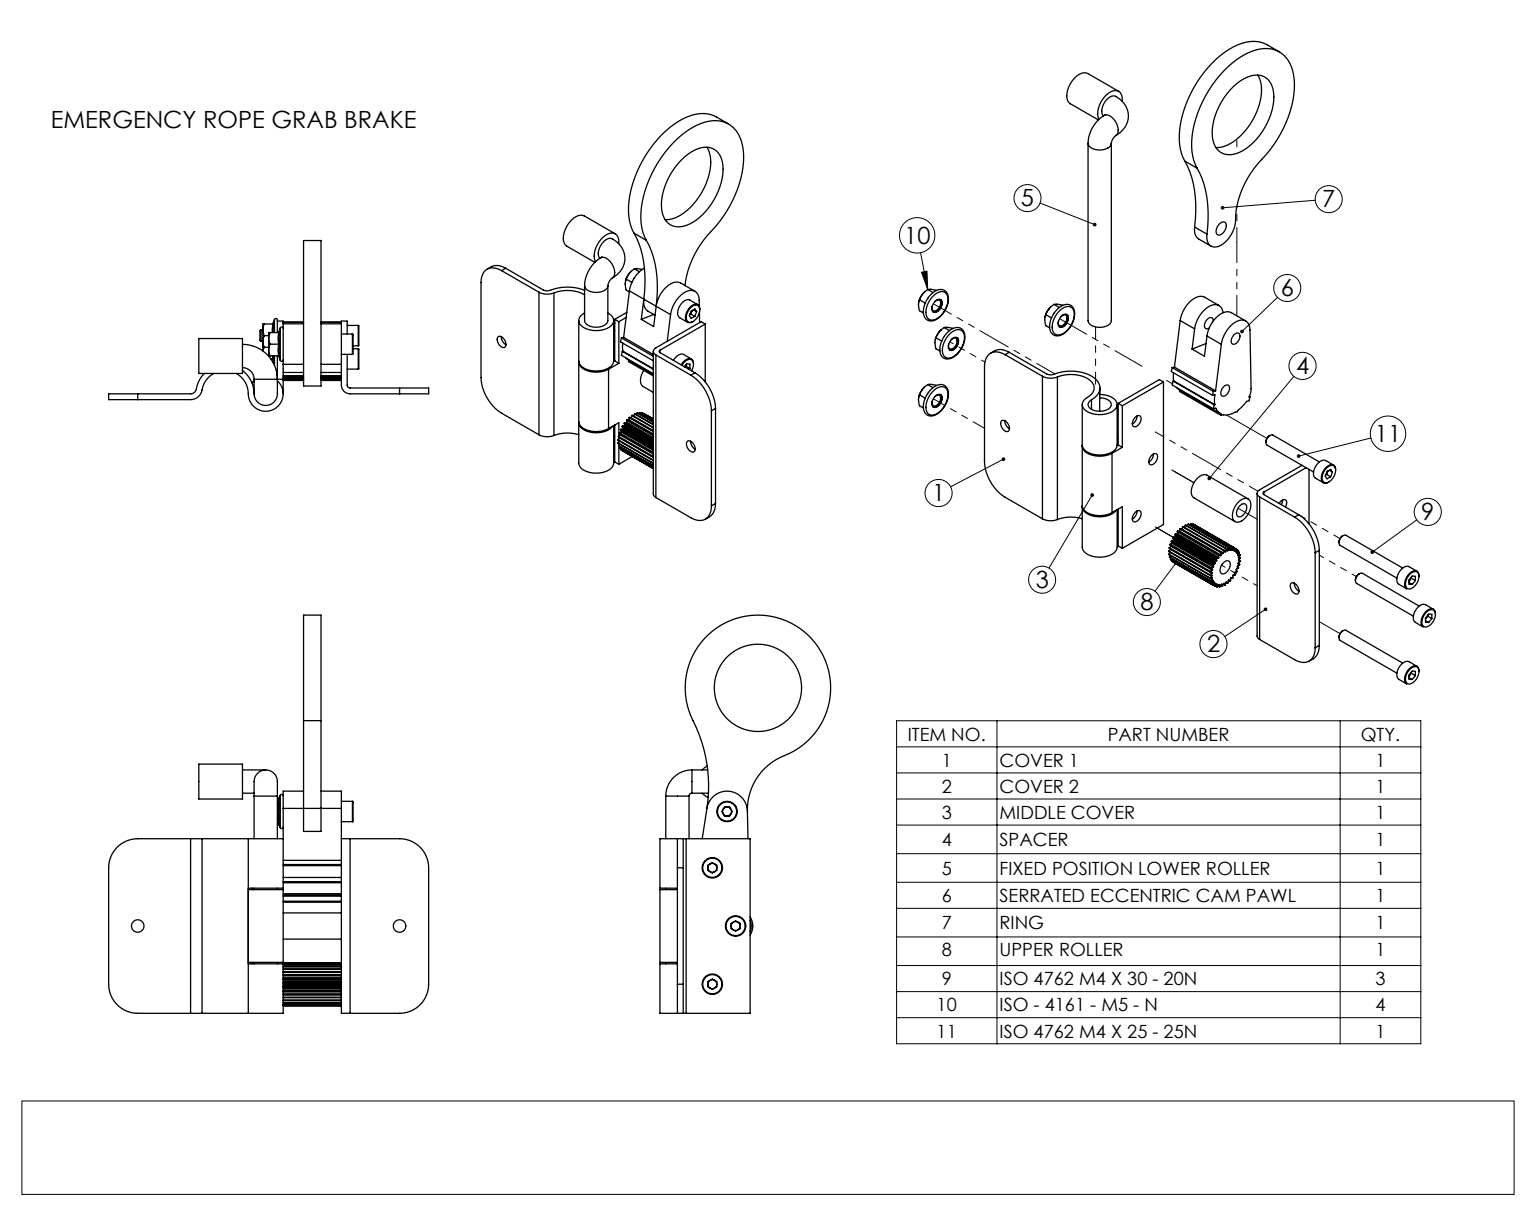
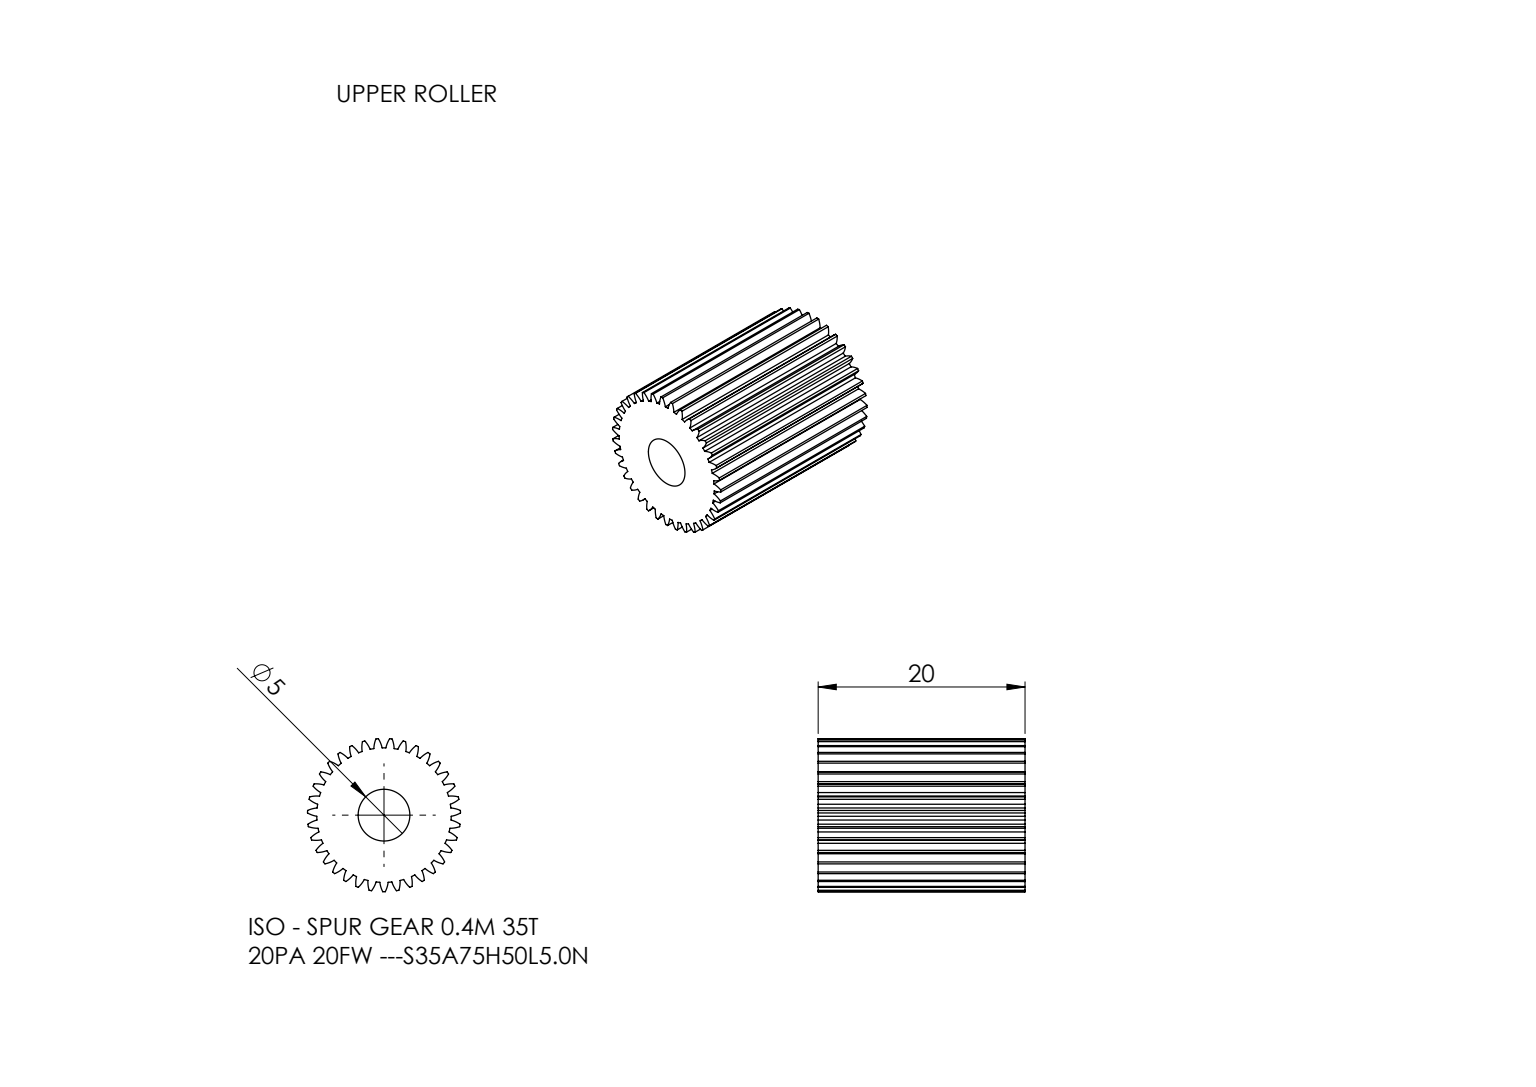
ISO-10303-21;
HEADER;
FILE_DESCRIPTION (('STEP AP214'),
    '1' );
FILE_NAME ('BR-598',
    '2026-10-03T20:08:58',
    ( '' ),
    ( '' ),
    'SwSTEP 2.0',
    'SolidWorks 2026',
    '' );
FILE_SCHEMA (( 'AUTOMOTIVE_DESIGN' ));
ENDSEC;

DATA;
#1 = FACE_OUTER_BOUND ( 'NONE', #4766, .T. ) ;
#2 = APPLICATION_CONTEXT ( 'automotive_design' ) ;
#3 = ORIENTED_EDGE ( 'NONE', *, *, #5317, .F. ) ;
#4 = CARTESIAN_POINT ( 'NONE',  ( 34.00000000000000000, 0.000000000000000000, -1.734723475976807094E-14 ) ) ;
#5 = ORIENTED_EDGE ( 'NONE', *, *, #5789, .T. ) ;
#6 = CARTESIAN_POINT ( 'NONE',  ( 33.00000000000001421, 39.34792583643766761, -10.06347054209568270 ) ) ;
#7 = AXIS2_PLACEMENT_3D ( 'NONE', #1534, #4440, #9440 ) ;
#9 = AXIS2_PLACEMENT_3D ( 'NONE', #3779, #3718, #5895 ) ;
#8 = SHAPE_REPRESENTATION_RELATIONSHIP ( 'NONE' , 'NONE' ,  #10094, #6187 ) ;
#10 = VECTOR ( 'NONE', #8821, 1000.000000000000000 ) ;
#11 = ADVANCED_FACE ( 'NONE', ( #11750 ), #8898, .T. ) ;
#12 = CARTESIAN_POINT ( 'NONE',  ( 19.99999999999997868, 5.670261409740700920, -3.175710400084609475 ) ) ;
#13 = CARTESIAN_POINT ( 'NONE',  ( 9.999999999999994671, -7.399010254356641170, 0.1210258481698957278 ) ) ;
#14 = FACE_OUTER_BOUND ( 'NONE', #4864, .T. ) ;
#15 = PLANE ( 'NONE',  #8371 ) ;
#16 = CARTESIAN_POINT ( 'NONE',  ( -3.999999999999991562, -0.3979232138631201288, 7.067642911889882029E-15 ) ) ;
#17 = DIRECTION ( 'NONE',  ( 0.000000000000000000, 0.000000000000000000, 1.000000000000000000 ) ) ;
#18 = DIRECTION ( 'NONE',  ( 1.140150527077241873E-30, 0.000000000000000000, -1.000000000000000000 ) ) ;
#19 = FACE_OUTER_BOUND ( 'NONE', #8393, .T. ) ;
#20 =( GEOMETRIC_REPRESENTATION_CONTEXT ( 3 ) GLOBAL_UNCERTAINTY_ASSIGNED_CONTEXT ( ( #3670 ) ) GLOBAL_UNIT_ASSIGNED_CONTEXT ( ( #5671, #4709, #1872 ) ) REPRESENTATION_CONTEXT ( 'NONE', 'WORKASPACE' ) );
#21 = ORIENTED_EDGE ( 'NONE', *, *, #12558, .T. ) ;
#22 = DIRECTION ( 'NONE',  ( -1.000000000000000000, 1.010728034814421376E-30, 1.090846720500930387E-30 ) ) ;
#23 = EDGE_CURVE ( 'NONE', #11067, #11603, #10115, .T. ) ;
#24 = LINE ( 'NONE', #10641, #9116 ) ;
#25 = CARTESIAN_POINT ( 'NONE',  ( 4.000000000000000000, -0.7890432684750908754, -0.04868663549882277369 ) ) ;
#27 = ADVANCED_FACE ( 'NONE', ( #3005 ), #10828, .T. ) ;
#26 = DIRECTION ( 'NONE',  ( 0.000000000000000000, 0.000000000000000000, 1.000000000000000000 ) ) ;
#28 = CARTESIAN_POINT ( 'NONE',  ( 19.99999999999999645, 0.000000000000000000, 0.000000000000000000 ) ) ;
#29 = ORIENTED_EDGE ( 'NONE', *, *, #11225, .F. ) ;
#30 = LINE ( 'NONE', #10838, #312 ) ;
#31 = CARTESIAN_POINT ( 'NONE',  ( 0.000000000000000000, -6.884685972239682705, 2.713134545806031195 ) ) ;
#32 = AXIS2_PLACEMENT_3D ( 'NONE', #10637, #3883, #7557 ) ;
#33 = DIRECTION ( 'NONE',  ( 1.000000000000000000, 1.081682119347366321E-16, -5.551115123125780237E-17 ) ) ;
#34 = ORIENTED_EDGE ( 'NONE', *, *, #4126, .T. ) ;
#35 = VERTEX_POINT ( 'NONE', #4203 ) ;
#36 = CARTESIAN_POINT ( 'NONE',  ( -3.333333333333346804, 2.694301256218253560, -3.300726591567095358 ) ) ;
#37 = ORIENTED_EDGE ( 'NONE', *, *, #5489, .T. ) ;
#38 = VERTEX_POINT ( 'NONE', #7300 ) ;
#39 = SHAPE_DEFINITION_REPRESENTATION ( #2484, #8378 ) ;
#40 = LINE ( 'NONE', #5122, #406 ) ;
#41 = VERTEX_POINT ( 'NONE', #145 ) ;
#42 = AXIS2_PLACEMENT_3D ( 'NONE', #12709, #3754, #3875 ) ;
#43 = FILL_AREA_STYLE ('',( #2962 ) ) ;
#44 = PLANE ( 'NONE',  #3777 ) ;
#45 = AXIS2_PLACEMENT_3D ( 'NONE', #142, #4066, #10040 ) ;
#46 = EDGE_CURVE ( 'NONE', #9407, #3079, #7991, .T. ) ;
#47 = VERTEX_POINT ( 'NONE', #5047 ) ;
#48 = DIRECTION ( 'NONE',  ( -0.000000000000000000, -1.000000000000000000, -0.000000000000000000 ) ) ;
#49 = CARTESIAN_POINT ( 'NONE',  ( 19.99999999999999645, -6.484265599627176968, 1.105616797298907716 ) ) ;
#50 = ORIENTED_EDGE ( 'NONE', *, *, #4393, .F. ) ;
#51 = ORIENTED_EDGE ( 'NONE', *, *, #132, .F. ) ;
#52 = AXIS2_PLACEMENT_3D ( 'NONE', #7977, #7092, #2061 ) ;
#53 = ORIENTED_EDGE ( 'NONE', *, *, #9830, .F. ) ;
#54 = DIRECTION ( 'NONE',  ( 7.272311470006191196E-31, 0.3513748240813434620, -0.9362348706397368714 ) ) ;
#55 = ORIENTED_EDGE ( 'NONE', *, *, #6653, .F. ) ;
#56 = ADVANCED_FACE ( 'NONE', ( #4070, #400 ), #9089, .T. ) ;
#57 = CARTESIAN_POINT ( 'NONE',  ( 19.99999999999999645, 0.000000000000000000, 0.000000000000000000 ) ) ;
#58 = ORIENTED_EDGE ( 'NONE', *, *, #11138, .F. ) ;
#59 = EDGE_CURVE ( 'NONE', #992, #4885, #7267, .T. ) ;
#60 = VECTOR ( 'NONE', #10370, 1000.000000000000000 ) ;
#61 = VECTOR ( 'NONE', #3554, 1000.000000000000000 ) ;
#62 = EDGE_CURVE ( 'NONE', #1807, #9471, #2410, .T. ) ;
#63 = CARTESIAN_POINT ( 'NONE',  ( 14.00000000000000000, 12.99999999999999822, 0.000000000000000000 ) ) ;
#64 = DIRECTION ( 'NONE',  ( -1.000000000000000000, 1.010728034814421376E-30, 1.090846720500930387E-30 ) ) ;
#65 = EDGE_CURVE ( 'NONE', #6211, #2771, #7241, .T. ) ;
#66 = EDGE_LOOP ( 'NONE', ( #746, #6032, #7828, #1571 ) ) ;
#67 = DIRECTION ( 'NONE',  ( -1.000000000000000000, 1.010728034814421376E-30, 1.090846720500930387E-30 ) ) ;
#68 = CIRCLE ( 'NONE', #2542, 6.499000000000009436 ) ;
#69 = ORIENTED_EDGE ( 'NONE', *, *, #11638, .T. ) ;
#70 = DIRECTION ( 'NONE',  ( 0.000000000000000000, 0.000000000000000000, 1.000000000000000000 ) ) ;
#71 = SHAPE_REPRESENTATION ( 'middle cover', ( #12422 ), #3113 ) ;
#72 = CARTESIAN_POINT ( 'NONE',  ( 2.000000000000001776, 1.773042676681341856, -3.469446951953614189E-15 ) ) ;
#73 = CARTESIAN_POINT ( 'NONE',  ( 19.99999999999999645, -2.385831757338583881, 6.045230171438861433 ) ) ;
#74 = VECTOR ( 'NONE', #10959, 1000.000000000000000 ) ;
#75 = CARTESIAN_POINT ( 'NONE',  ( -11.83215956619923226, -30.00000000000000000, -4.336808689942017736E-16 ) ) ;
#76 = CARTESIAN_POINT ( 'NONE',  ( -2.000000000000008882, -3.464101615137750390, -8.673617379884035472E-15 ) ) ;
#77 = DIRECTION ( 'NONE',  ( 0.000000000000000000, 0.000000000000000000, 1.000000000000000000 ) ) ;
#78 = CARTESIAN_POINT ( 'NONE',  ( 19.99999999999997868, -2.171317488608451196, -7.074275960383738848 ) ) ;
#79 = LINE ( 'NONE', #4007, #1843 ) ;
#80 = CARTESIAN_POINT ( 'NONE',  ( -16.99999999999999289, 30.00000000000000000, 25.00000000000007105 ) ) ;
#81 = AXIS2_PLACEMENT_3D ( 'NONE', #653, #10630, #1876 ) ;
#82 = ORIENTED_EDGE ( 'NONE', *, *, #340, .T. ) ;
#83 = ORIENTED_EDGE ( 'NONE', *, *, #1095, .T. ) ;
#84 = CARTESIAN_POINT ( 'NONE',  ( 3.469446951953614189E-14, -3.469446951953614189E-15, -4.694516984716123886 ) ) ;
#85 = FACE_OUTER_BOUND ( 'NONE', #4807, .T. ) ;
#86 = LINE ( 'NONE', #3133, #9986 ) ;
#87 = VERTEX_POINT ( 'NONE', #3260 ) ;
#88 = AXIS2_PLACEMENT_3D ( 'NONE', #6205, #12269, #12210 ) ;
#89 = EDGE_CURVE ( 'NONE', #11132, #9471, #8961, .T. ) ;
#90 = FACE_OUTER_BOUND ( 'NONE', #10199, .T. ) ;
#91 = LINE ( 'NONE', #9864, #6054 ) ;
#92 = CARTESIAN_POINT ( 'NONE',  ( 40.00000000000006395, 1.290960574571364216E-15, -20.00000000000000000 ) ) ;
#93 = VERTEX_POINT ( 'NONE', #9152 ) ;
#94 = ORIENTED_EDGE ( 'NONE', *, *, #6721, .T. ) ;
#95 = CARTESIAN_POINT ( 'NONE',  ( 20.00000000000000000, 39.49790820824818383, -24.06186359251417883 ) ) ;
#96 = EDGE_LOOP ( 'NONE', ( #11303, #3914, #11621, #9750 ) ) ;
#97 = AXIS2_PLACEMENT_3D ( 'NONE', #1483, #11545, #8437 ) ;
#98 = ORIENTED_EDGE ( 'NONE', *, *, #5230, .F. ) ;
#99 = SHAPE_DEFINITION_REPRESENTATION ( #6268, #1377 ) ;
#100 = DIRECTION ( 'NONE',  ( 0.000000000000000000, -0.9909497617679331460, -0.1342332658176667304 ) ) ;
#101 = ORIENTED_EDGE ( 'NONE', *, *, #1479, .F. ) ;
#102 = DIRECTION ( 'NONE',  ( -1.000000000000000000, 1.010728034814421376E-30, 1.090846720500930387E-30 ) ) ;
#103 = ORIENTED_EDGE ( 'NONE', *, *, #2776, .T. ) ;
#104 = FACE_OUTER_BOUND ( 'NONE', #9795, .T. ) ;
#105 = CARTESIAN_POINT ( 'NONE',  ( 9.999999999999994671, -7.301715115245761112, -1.202063382601588959 ) ) ;
#106 = CONICAL_SURFACE ( 'NONE', #7315, 1.535500000000000087, 1.047197551196590748 ) ;
#107 = CIRCLE ( 'NONE', #5659, 4.000000000000001776 ) ;
#108 = ORIENTED_EDGE ( 'NONE', *, *, #10644, .F. ) ;
#109 = ADVANCED_FACE ( 'NONE', ( #2146 ), #3325, .T. ) ;
#110 = ORIENTED_EDGE ( 'NONE', *, *, #895, .F. ) ;
#111 = EDGE_CURVE ( 'NONE', #3787, #7514, #12202, .T. ) ;
#112 = EDGE_CURVE ( 'NONE', #3836, #11042, #11228, .T. ) ;
#113 = ORIENTED_EDGE ( 'NONE', *, *, #3942, .T. ) ;
#114 = DIRECTION ( 'NONE',  ( -1.000000000000000000, 1.010728034814421376E-30, 1.090846720500930387E-30 ) ) ;
#115 = DIRECTION ( 'NONE',  ( 0.000000000000000000, -1.530455820933490821E-32, 1.000000000000000000 ) ) ;
#116 = ORIENTED_EDGE ( 'NONE', *, *, #9811, .T. ) ;
#117 = AXIS2_PLACEMENT_3D ( 'NONE', #8062, #12074, #12010 ) ;
#118 = DIRECTION ( 'NONE',  ( 1.238279320584846685E-16, -0.9554649393887558739, 0.2951046417778634412 ) ) ;
#119 = ORIENTED_EDGE ( 'NONE', *, *, #7545, .T. ) ;
#120 = EDGE_CURVE ( 'NONE', #10609, #7454, #4588, .T. ) ;
#121 = FACE_OUTER_BOUND ( 'NONE', #12151, .T. ) ;
#122 = CARTESIAN_POINT ( 'NONE',  ( 19.99999999999999645, -5.610543508060446882, 3.433640984893234549 ) ) ;
#123 = CARTESIAN_POINT ( 'NONE',  ( 19.99999999999999645, -4.155687294075553595, -5.098857909653601084 ) ) ;
#124 = VECTOR ( 'NONE', #5391, 1000.000000000000000 ) ;
#125 = VERTEX_POINT ( 'NONE', #8190 ) ;
#126 = FACE_OUTER_BOUND ( 'NONE', #189, .T. ) ;
#127 = ORIENTED_EDGE ( 'NONE', *, *, #89, .F. ) ;
#128 = CARTESIAN_POINT ( 'NONE',  ( 19.99999999999999645, 0.000000000000000000, 0.000000000000000000 ) ) ;
#129 = CARTESIAN_POINT ( 'NONE',  ( 9.999999999999998224, 7.100173756228433497, 2.085073771204572157 ) ) ;
#130 = CIRCLE ( 'NONE', #8361, 7.400000000000011902 ) ;
#131 = DIRECTION ( 'NONE',  ( 0.000000000000000000, -1.177425296209236209E-30, -1.000000000000000000 ) ) ;
#132 = EDGE_CURVE ( 'NONE', #3832, #6132, #1903, .T. ) ;
#133 = CIRCLE ( 'NONE', #4662, 7.400000000000011902 ) ;
#134 = CARTESIAN_POINT ( 'NONE',  ( 0.000000000000000000, 4.192831774278975132, 4.965597920955404199 ) ) ;
#135 = CARTESIAN_POINT ( 'NONE',  ( 40.00000000000000711, 9.597108420813798446, -18.39576936187866352 ) ) ;
#136 = DIRECTION ( 'NONE',  ( 1.000000000000000000, 0.000000000000000000, 0.000000000000000000 ) ) ;
#137 = DIRECTION ( 'NONE',  ( 1.000000000000000000, -1.010728034814421376E-30, -1.090846720500930387E-30 ) ) ;
#138 = PRODUCT_DEFINITION_FORMATION_WITH_SPECIFIED_SOURCE ( 'ANY', '', #5241, .NOT_KNOWN. ) ;
#139 = DIRECTION ( 'NONE',  ( 0.000000000000000000, 0.000000000000000000, -1.000000000000000000 ) ) ;
#140 = CIRCLE ( 'NONE', #5087, 10.00000000000002309 ) ;
#141 = ADVANCED_FACE ( 'NONE', ( #9022 ), #11990, .F. ) ;
#142 = CARTESIAN_POINT ( 'NONE',  ( 14.00000000000000000, 13.00000000000000000, 0.000000000000000000 ) ) ;
#143 = EDGE_CURVE ( 'NONE', #5907, #8271, #10318, .T. ) ;
#144 = VERTEX_POINT ( 'NONE', #12137 ) ;
#145 = CARTESIAN_POINT ( 'NONE',  ( 19.99999999999997868, 0.6915992404090851586, -6.462096524400249287 ) ) ;
#146 = CARTESIAN_POINT ( 'NONE',  ( 0.000000000000000000, 4.772487208025128602, 4.411390579991361527 ) ) ;
#147 = CARTESIAN_POINT ( 'NONE',  ( 19.99999999999999645, -5.651611091574833878, 4.776954267060571802 ) ) ;
#148 = CARTESIAN_POINT ( 'NONE',  ( 14.00000000000000000, -13.00000000000000000, 0.000000000000000000 ) ) ;
#149 = CARTESIAN_POINT ( 'NONE',  ( 20.00000000000000355, 19.99999999999999645, -9.850000000000008527 ) ) ;
#150 = ORIENTED_EDGE ( 'NONE', *, *, #8938, .F. ) ;
#151 = CIRCLE ( 'NONE', #11268, 2.800000000000003375 ) ;
#152 = FACE_OUTER_BOUND ( 'NONE', #1535, .T. ) ;
#153 = CYLINDRICAL_SURFACE ( 'NONE', #2365, 2.149999999999999023 ) ;
#154 = EDGE_CURVE ( 'NONE', #6728, #2957, #12005, .T. ) ;
#155 = ORIENTED_EDGE ( 'NONE', *, *, #11867, .F. ) ;
#156 = VERTEX_POINT ( 'NONE', #5173 ) ;
#157 = DIRECTION ( 'NONE',  ( 0.000000000000000000, -1.530455820933490821E-32, 1.000000000000000000 ) ) ;
#158 = ORIENTED_EDGE ( 'NONE', *, *, #7731, .T. ) ;
#159 = ORIENTED_EDGE ( 'NONE', *, *, #9670, .T. ) ;
#160 = APPLICATION_PROTOCOL_DEFINITION ( 'draft international standard', 'automotive_design', 1998, #5024 ) ;
#161 = DIRECTION ( 'NONE',  ( 0.000000000000000000, 0.000000000000000000, 1.000000000000000000 ) ) ;
#162 = ORIENTED_EDGE ( 'NONE', *, *, #10787, .F. ) ;
#163 = CARTESIAN_POINT ( 'NONE',  ( 4.000000000000003553, 1.942890293094023946E-16, 3.500000000000003997 ) ) ;
#164 = EDGE_CURVE ( 'NONE', #2848, #3887, #6852, .T. ) ;
#165 = CARTESIAN_POINT ( 'NONE',  ( 14.00000000000000000, -30.00000000000000000, 0.000000000000000000 ) ) ;
#166 = EDGE_LOOP ( 'NONE', ( #3559, #613, #8519, #6620, #10979 ) ) ;
#167 = CARTESIAN_POINT ( 'NONE',  ( 0.000000000000000000, 4.772487208025201433, -4.411390579991299354 ) ) ;
#168 = DIRECTION ( 'NONE',  ( -1.000000000000000000, 1.010728034814421376E-30, 1.090846720500930387E-30 ) ) ;
#169 =( REPRESENTATION_RELATIONSHIP ('NONE','NONE', #10018, #9199 ) REPRESENTATION_RELATIONSHIP_WITH_TRANSFORMATION ( #7317 )SHAPE_REPRESENTATION_RELATIONSHIP( ) );
#170 = CARTESIAN_POINT ( 'NONE',  ( 20.00000000000000355, 10.25912655421750230, -11.14847175327133577 ) ) ;
#171 = AXIS2_PLACEMENT_3D ( 'NONE', #7633, #11626, #11439 ) ;
#172 = ORIENTED_EDGE ( 'NONE', *, *, #1630, .T. ) ;
#173 = ORIENTED_EDGE ( 'NONE', *, *, #5262, .T. ) ;
#174 = ORIENTED_EDGE ( 'NONE', *, *, #9059, .T. ) ;
#175 = VERTEX_POINT ( 'NONE', #5295 ) ;
#176 = FACE_OUTER_BOUND ( 'NONE', #7657, .T. ) ;
#177 = CARTESIAN_POINT ( 'NONE',  ( 4.203935335434870524, 1.640780671294068238, -3.598452447879444627 ) ) ;
#178 = ORIENTED_EDGE ( 'NONE', *, *, #3075, .F. ) ;
#179 = FACE_OUTER_BOUND ( 'NONE', #3393, .T. ) ;
#180 = CONICAL_SURFACE ( 'NONE', #8811, 4.000000000000000000, 0.8911886515913786111 ) ;
#181 = ORIENTED_EDGE ( 'NONE', *, *, #9473, .F. ) ;
#182 = CARTESIAN_POINT ( 'NONE',  ( 3.122502256758252770E-14, -4.862606272033112909, -3.745885042887444616 ) ) ;
#183 = EDGE_CURVE ( 'NONE', #1508, #4176, #5201, .T. ) ;
#184 = ADVANCED_FACE ( 'NONE', ( #12327 ), #9395, .T. ) ;
#185 = CARTESIAN_POINT ( 'NONE',  ( 15.00000000000003375, -12.49999999999999645, 3.994800001834461867E-31 ) ) ;
#186 = AXIS2_PLACEMENT_3D ( 'NONE', #11743, #4909, #6785 ) ;
#187 = AXIS2_PLACEMENT_3D ( 'NONE', #3419, #6498, #628 ) ;
#188 = FACE_OUTER_BOUND ( 'NONE', #3903, .T. ) ;
#189 = EDGE_LOOP ( 'NONE', ( #7813, #4813, #3733, #12234, #6794, #9118 ) ) ;
#190 = FACE_OUTER_BOUND ( 'NONE', #6817, .T. ) ;
#191 = ORIENTED_EDGE ( 'NONE', *, *, #10270, .T. ) ;
#192 = PLANE ( 'NONE',  #6009 ) ;
#193 =( NAMED_UNIT ( * ) PLANE_ANGLE_UNIT ( ) SI_UNIT ( $, .RADIAN. ) );
#194 = FACE_OUTER_BOUND ( 'NONE', #7754, .T. ) ;
#195 = AXIS2_PLACEMENT_3D ( 'NONE', #7539, #2660, #4452 ) ;
#196 = AXIS2_PLACEMENT_3D ( 'NONE', #1167, #8956, #10887 ) ;
#197 = CIRCLE ( 'NONE', #2043, 2.800000000000002931 ) ;
#198 = DIRECTION ( 'NONE',  ( 1.000000000000000000, 1.849040895279789448E-31, -6.938893903907224680E-17 ) ) ;
#199 = AXIS2_PLACEMENT_3D ( 'NONE', #4415, #11118, #3403 ) ;
#200 = CARTESIAN_POINT ( 'NONE',  ( 2.000000000000001776, 0.000000000000000000, 0.000000000000000000 ) ) ;
#201 = DIRECTION ( 'NONE',  ( 0.000000000000000000, 0.4999999999999989453, -0.8660254037844392627 ) ) ;
#202 = DIRECTION ( 'NONE',  ( -1.000000000000000000, 1.010728034814421376E-30, 1.090846720500930387E-30 ) ) ;
#203 = CARTESIAN_POINT ( 'NONE',  ( 15.00000000000003375, 30.00000000000001776, -9.742497179615118866E-31 ) ) ;
#204 = CIRCLE ( 'NONE', #7, 6.499000000000010324 ) ;
#205 = AXIS2_PLACEMENT_3D ( 'NONE', #5168, #9083, #12128 ) ;
#206 = CARTESIAN_POINT ( 'NONE',  ( 0.000000000000000000, -1.623118704078857499, -6.293050665016890477 ) ) ;
#207 = ORIENTED_EDGE ( 'NONE', *, *, #11487, .T. ) ;
#208 = CARTESIAN_POINT ( 'NONE',  ( 0.000000000000000000, 0.000000000000000000, 0.000000000000000000 ) ) ;
#209 = COLOUR_RGB ( '', 0.66274510, 0.83137255, 0.94901961) ;
#210 = PRESENTATION_LAYER_ASSIGNMENT (  '', '', ( #5766 ) ) ;
#211 = CARTESIAN_POINT ( 'NONE',  ( 27.00000000000000355, 39.34792583643766051, -14.91347054209568945 ) ) ;
#212 = CARTESIAN_POINT ( 'NONE',  ( 2.000000000000001776, -1.773042676681341856, 3.469446951953614189E-15 ) ) ;
#213 = EDGE_CURVE ( 'NONE', #4292, #815, #7867, .T. ) ;
#214 = CARTESIAN_POINT ( 'NONE',  ( 0.000000000000000000, 0.000000000000000000, 0.000000000000000000 ) ) ;
#215 = ORIENTED_EDGE ( 'NONE', *, *, #9401, .F. ) ;
#216 = CARTESIAN_POINT ( 'NONE',  ( 40.00000000000000000, 39.34792583643765340, -17.06347054209567560 ) ) ;
#217 = EDGE_CURVE ( 'NONE', #10195, #4167, #2330, .T. ) ;
#218 = CARTESIAN_POINT ( 'NONE',  ( 2.000000000000001776, -0.8865213383406691516, 1.535500000000002085 ) ) ;
#219 = ORIENTED_EDGE ( 'NONE', *, *, #11430, .T. ) ;
#220 = ADVANCED_FACE ( 'NONE', ( #2602 ), #12455, .T. ) ;
#221 = DIRECTION ( 'NONE',  ( 0.000000000000000000, 0.000000000000000000, 1.000000000000000000 ) ) ;
#222 = VERTEX_POINT ( 'NONE', #588 ) ;
#223 = EDGE_LOOP ( 'NONE', ( #680, #8634, #6232, #8801 ) ) ;
#224 = APPLICATION_PROTOCOL_DEFINITION ( 'draft international standard', 'automotive_design', 1998, #2906 ) ;
#225 = CYLINDRICAL_SURFACE ( 'NONE', #8627, 4.000000000000008882 ) ;
#226 = ORIENTED_EDGE ( 'NONE', *, *, #11853, .T. ) ;
#227 =( NAMED_UNIT ( * ) PLANE_ANGLE_UNIT ( ) SI_UNIT ( $, .RADIAN. ) );
#228 = CARTESIAN_POINT ( 'NONE',  ( 19.99999999999997868, 6.146182963951697609, -2.112211157443803611 ) ) ;
#229 = VERTEX_POINT ( 'NONE', #7547 ) ;
#230 = CARTESIAN_POINT ( 'NONE',  ( 9.999999999999980460, -5.492355906873422455, 4.959236492871922586 ) ) ;
#231 = CARTESIAN_POINT ( 'NONE',  ( 40.00000000000000711, 10.63631887905126128, -9.927230231572499619 ) ) ;
#232 = DIRECTION ( 'NONE',  ( 1.158639454543359513E-30, -0.1785568947986227173, -0.9839295885986321100 ) ) ;
#233 = DIRECTION ( 'NONE',  ( 0.000000000000000000, 0.8660254037844380415, -0.5000000000000012212 ) ) ;
#234 = CIRCLE ( 'NONE', #8869, 6.000000000000000888 ) ;
#235 = VERTEX_POINT ( 'NONE', #4529 ) ;
#236 = ORIENTED_EDGE ( 'NONE', *, *, #12303, .F. ) ;
#237 = EDGE_LOOP ( 'NONE', ( #1805, #3324, #10150, #7771, #10592, #866 ) ) ;
#238 = ORIENTED_EDGE ( 'NONE', *, *, #6687, .T. ) ;
#239 = CIRCLE ( 'NONE', #9478, 4.000000000000001776 ) ;
#240 = DIRECTION ( 'NONE',  ( -4.930380657631325535E-31, -1.000000000000000000, -1.177425296209239362E-30 ) ) ;
#241 = AXIS2_PLACEMENT_3D ( 'NONE', #12258, #11351, #9391 ) ;
#242 = CARTESIAN_POINT ( 'NONE',  ( 0.000000000000000000, 0.000000000000000000, 0.000000000000000000 ) ) ;
#243 = ORIENTED_EDGE ( 'NONE', *, *, #11135, .T. ) ;
#244 = CARTESIAN_POINT ( 'NONE',  ( -10.00000000000000178, 0.000000000000000000, 0.000000000000000000 ) ) ;
#245 = VERTEX_POINT ( 'NONE', #10303 ) ;
#246 = CARTESIAN_POINT ( 'NONE',  ( 19.99999999999999645, -4.155687294075553595, -5.098857909653601084 ) ) ;
#247 = AXIS2_PLACEMENT_3D ( 'NONE', #6312, #11214, #8436 ) ;
#248 = CARTESIAN_POINT ( 'NONE',  ( 0.000000000000000000, 0.000000000000000000, 0.000000000000000000 ) ) ;
#249 = LINE ( 'NONE', #7281, #6377 ) ;
#250 = ORIENTED_EDGE ( 'NONE', *, *, #9565, .F. ) ;
#251 = DIRECTION ( 'NONE',  ( -1.000000000000000000, -0.000000000000000000, -0.000000000000000000 ) ) ;
#252 = ORIENTED_EDGE ( 'NONE', *, *, #804, .T. ) ;
#253 = CARTESIAN_POINT ( 'NONE',  ( 0.000000000000000000, 0.000000000000000000, 0.000000000000000000 ) ) ;
#254 = EDGE_CURVE ( 'NONE', #6132, #11730, #871, .T. ) ;
#255 =( LENGTH_UNIT ( ) NAMED_UNIT ( * ) SI_UNIT ( .MILLI., .METRE. ) );
#256 = AXIS2_PLACEMENT_3D ( 'NONE', #10439, #11422, #1428 ) ;
#257 = CARTESIAN_POINT ( 'NONE',  ( 0.000000000000000000, -0.4733669331951463888, -6.481737787550307495 ) ) ;
#258 = AXIS2_PLACEMENT_3D ( 'NONE', #11847, #1979, #9819 ) ;
#259 = CARTESIAN_POINT ( 'NONE',  ( -18.00000000000000355, 29.99999999999998224, 3.000000000000008438 ) ) ;
#260 = CARTESIAN_POINT ( 'NONE',  ( 33.00000000000001421, 39.34792583643766761, -17.06347054209568270 ) ) ;
#261 = CARTESIAN_POINT ( 'NONE',  ( -35.00000000000006395, 30.00000000000000000, 2.000000000000006661 ) ) ;
#262 = CIRCLE ( 'NONE', #8491, 7.400000000000009237 ) ;
#263 = CARTESIAN_POINT ( 'NONE',  ( -15.00000000000003375, 19.99999999999998934, 12.00000000000002842 ) ) ;
#264 = AXIS2_PLACEMENT_3D ( 'NONE', #2269, #10097, #5222 ) ;
#265 = AXIS2_PLACEMENT_3D ( 'NONE', #2707, #625, #8413 ) ;
#266 = DIRECTION ( 'NONE',  ( -1.000000000000000000, 1.006188713385347367E-17, 3.844790828812615713E-17 ) ) ;
#267 = DIRECTION ( 'NONE',  ( -1.000000000000000000, 1.010728034814421376E-30, 1.090846720500930387E-30 ) ) ;
#268 = EDGE_CURVE ( 'NONE', #6675, #6031, #2672, .T. ) ;
#269 = EDGE_CURVE ( 'NONE', #1961, #1191, #3966, .T. ) ;
#270 = PRODUCT_RELATED_PRODUCT_CATEGORY ( 'part', '', ( #4538 ) ) ;
#271 = VERTEX_POINT ( 'NONE', #9524 ) ;
#272 = DIRECTION ( 'NONE',  ( 0.000000000000000000, 0.9195277725514489076, 0.3930250316539277144 ) ) ;
#273 = CARTESIAN_POINT ( 'NONE',  ( 0.000000000000000000, 30.00000000000000000, 0.000000000000000000 ) ) ;
#274 = CARTESIAN_POINT ( 'NONE',  ( -3.999999999999628741, -1.658469974638250077, -3.531532913077053415 ) ) ;
#275 = CYLINDRICAL_SURFACE ( 'NONE', #8773, 2.800000000000003819 ) ;
#276 = VERTEX_POINT ( 'NONE', #717 ) ;
#277 = DIRECTION ( 'NONE',  ( -0.000000000000000000, -0.9883022714608525883, 0.1525077710325583313 ) ) ;
#278 = AXIS2_PLACEMENT_3D ( 'NONE', #6450, #2458, #6380 ) ;
#279 = CARTESIAN_POINT ( 'NONE',  ( -18.00000000000000355, 29.99999999999998224, 3.000000000000008438 ) ) ;
#280 =( LENGTH_UNIT ( ) NAMED_UNIT ( * ) SI_UNIT ( .MILLI., .METRE. ) );
#281 = AXIS2_PLACEMENT_3D ( 'NONE', #5557, #12328, #3506 ) ;
#282 = EDGE_LOOP ( 'NONE', ( #8241, #11601, #3963, #2292 ) ) ;
#283 = CARTESIAN_POINT ( 'NONE',  ( 2.000000000000001776, 1.773042676681341856, -3.469446951953614189E-15 ) ) ;
#284 = ORIENTED_EDGE ( 'NONE', *, *, #4561, .F. ) ;
#285 = ORIENTED_EDGE ( 'NONE', *, *, #3237, .F. ) ;
#286 = DIRECTION ( 'NONE',  ( -1.000000000000000000, 1.010728034814421376E-30, 1.090846720500930387E-30 ) ) ;
#287 = ORIENTED_EDGE ( 'NONE', *, *, #3604, .F. ) ;
#288 = AXIS2_PLACEMENT_3D ( 'NONE', #9402, #7554, #2747 ) ;
#289 = DIRECTION ( 'NONE',  ( 0.000000000000000000, 0.000000000000000000, 1.000000000000000000 ) ) ;
#290 = DIRECTION ( 'NONE',  ( 1.000000000000000000, -1.010728034814421376E-30, -1.090846720500930387E-30 ) ) ;
#291 = VERTEX_POINT ( 'NONE', #5614 ) ;
#292 = AXIS2_PLACEMENT_3D ( 'NONE', #6749, #3786, #3026 ) ;
#293 = CARTESIAN_POINT ( 'NONE',  ( 9.999999999999998224, 3.019282868015183752, -6.756029230465944835 ) ) ;
#294 = DIRECTION ( 'NONE',  ( 0.000000000000000000, 0.000000000000000000, -1.000000000000000000 ) ) ;
#295 = DIRECTION ( 'NONE',  ( 0.000000000000000000, -1.530455820933490821E-32, 1.000000000000000000 ) ) ;
#296 = EDGE_CURVE ( 'NONE', #2105, #6027, #1281, .T. ) ;
#297 = FACE_OUTER_BOUND ( 'NONE', #12054, .T. ) ;
#298 = ORIENTED_EDGE ( 'NONE', *, *, #6646, .F. ) ;
#299 = AXIS2_PLACEMENT_3D ( 'NONE', #10361, #5481, #9387 ) ;
#300 = AXIS2_PLACEMENT_3D ( 'NONE', #8481, #819, #7524 ) ;
#301 = EDGE_LOOP ( 'NONE', ( #811, #8757, #4299, #181 ) ) ;
#302 = VERTEX_POINT ( 'NONE', #12517 ) ;
#303 = VERTEX_POINT ( 'NONE', #7427 ) ;
#304 = EDGE_CURVE ( 'NONE', #11281, #1954, #7365, .T. ) ;
#305 = DIRECTION ( 'NONE',  ( -0.000000000000000000, -1.000000000000000000, -0.000000000000000000 ) ) ;
#306 = EDGE_CURVE ( 'NONE', #7136, #2489, #7613, .T. ) ;
#307 = FACE_OUTER_BOUND ( 'NONE', #3872, .T. ) ;
#308 = ORIENTED_EDGE ( 'NONE', *, *, #4239, .F. ) ;
#309 = CARTESIAN_POINT ( 'NONE',  ( 14.00000000000000000, 45.63999999999998636, -5.000000000000001776 ) ) ;
#310 = ORIENTED_EDGE ( 'NONE', *, *, #2739, .F. ) ;
#311 = VECTOR ( 'NONE', #12495, 1000.000000000000000 ) ;
#312 = VECTOR ( 'NONE', #2087, 1000.000000000000000 ) ;
#313 = CARTESIAN_POINT ( 'NONE',  ( -2.687328764639639544, 3.067272167851286646, -0.05923475698270460471 ) ) ;
#314 = CARTESIAN_POINT ( 'NONE',  ( 3.436319922986161401, -2.634841920958475026, -3.531542292954823470 ) ) ;
#315 = DIRECTION ( 'NONE',  ( 0.000000000000000000, -1.000000000000000000, 0.000000000000000000 ) ) ;
#316 = ORIENTED_EDGE ( 'NONE', *, *, #9501, .T. ) ;
#317 = EDGE_CURVE ( 'NONE', #3010, #5117, #3561, .T. ) ;
#318 = DIRECTION ( 'NONE',  ( 0.000000000000000000, -1.000000000000000000, 8.560894001270036306E-16 ) ) ;
#319 = ORIENTED_EDGE ( 'NONE', *, *, #10446, .F. ) ;
#320 = AXIS2_PLACEMENT_3D ( 'NONE', #11362, #2607, #1756 ) ;
#321 = DIRECTION ( 'NONE',  ( 0.000000000000000000, -1.000000000000000000, 0.000000000000000000 ) ) ;
#322 = SHAPE_REPRESENTATION_RELATIONSHIP ( 'NONE' , 'NONE' ,  #4436, #9258 ) ;
#323 = EDGE_CURVE ( 'NONE', #2041, #8095, #6021, .T. ) ;
#324 = FACE_BOUND ( 'NONE', #7382, .T. ) ;
#325 = CYLINDRICAL_SURFACE ( 'NONE', #7247, 2.800000000000003819 ) ;
#326 = EDGE_CURVE ( 'NONE', #1272, #144, #5806, .T. ) ;
#327 = CYLINDRICAL_SURFACE ( 'NONE', #7553, 6.499000000000010324 ) ;
#328 = DIRECTION ( 'NONE',  ( 1.000000000000000000, 1.849040895279789448E-31, -6.938893903907224680E-17 ) ) ;
#329 = DIRECTION ( 'NONE',  ( 2.218671295934092637E-31, -0.8345732537213080837, 0.5508969814520944253 ) ) ;
#330 = CYLINDRICAL_SURFACE ( 'NONE', #9243, 2.800000000000003819 ) ;
#331 = CARTESIAN_POINT ( 'NONE',  ( 15.00000000000003375, 12.50000000000000000, -4.062508476441825628E-31 ) ) ;
#332 = AXIS2_PLACEMENT_3D ( 'NONE', #551, #4484, #8402 ) ;
#333 = EDGE_CURVE ( 'NONE', #5304, #561, #531, .T. ) ;
#334 = AXIS2_PLACEMENT_3D ( 'NONE', #8900, #11752, #2944 ) ;
#335 = VERTEX_POINT ( 'NONE', #4396 ) ;
#336 = DIRECTION ( 'NONE',  ( -2.218671295934093250E-30, 5.551115123125776539E-17, 1.000000000000000000 ) ) ;
#337 = CARTESIAN_POINT ( 'NONE',  ( 0.000000000000000000, 6.557268578288196537, 0.5199208220222142351 ) ) ;
#338 = DIRECTION ( 'NONE',  ( 0.000000000000000000, 0.000000000000000000, 1.000000000000000000 ) ) ;
#339 = CARTESIAN_POINT ( 'NONE',  ( 19.99999999999999645, 6.018220532833773007, 2.453165835849278942 ) ) ;
#340 = EDGE_CURVE ( 'NONE', #9694, #2491, #8482, .T. ) ;
#341 = DIRECTION ( 'NONE',  ( 0.000000000000000000, -5.551115123125770376E-17, -1.000000000000000000 ) ) ;
#342 = EDGE_CURVE ( 'NONE', #10168, #10108, #1081, .T. ) ;
#343 = CIRCLE ( 'NONE', #6939, 6.499000000000008548 ) ;
#344 = DIRECTION ( 'NONE',  ( 0.000000000000000000, 0.000000000000000000, -1.000000000000000000 ) ) ;
#345 = EDGE_CURVE ( 'NONE', #11393, #10993, #9909, .T. ) ;
#346 = ORIENTED_EDGE ( 'NONE', *, *, #1046, .T. ) ;
#347 = FACE_OUTER_BOUND ( 'NONE', #4727, .T. ) ;
#348 = ORIENTED_EDGE ( 'NONE', *, *, #8128, .T. ) ;
#349 = VERTEX_POINT ( 'NONE', #907 ) ;
#350 = VECTOR ( 'NONE', #4831, 1000.000000000000000 ) ;
#351 = ORIENTED_EDGE ( 'NONE', *, *, #8169, .F. ) ;
#352 = CIRCLE ( 'NONE', #6535, 2.149999999999994138 ) ;
#353 = CARTESIAN_POINT ( 'NONE',  ( 0.000000000000000000, 2.649444137877595473, 6.020675595748707032 ) ) ;
#354 = AXIS2_PLACEMENT_3D ( 'NONE', #7776, #2780, #817 ) ;
#355 = DIRECTION ( 'NONE',  ( -1.000000000000000000, 1.010728034814421376E-30, 1.090846720500930387E-30 ) ) ;
#356 = DIRECTION ( 'NONE',  ( -1.000000000000000000, 1.010728034814421376E-30, 1.090846720500930387E-30 ) ) ;
#357 = LINE ( 'NONE', #2369, #4310 ) ;
#358 = DIRECTION ( 'NONE',  ( 0.000000000000000000, 0.000000000000000000, 1.000000000000000000 ) ) ;
#359 = CARTESIAN_POINT ( 'NONE',  ( 0.1404048886732742751, 4.699864953788060795, -3.686887068327044048 ) ) ;
#360 = EDGE_CURVE ( 'NONE', #9103, #2750, #9300, .T. ) ;
#361 = LINE ( 'NONE', #555, #3321 ) ;
#362 = ORIENTED_EDGE ( 'NONE', *, *, #10996, .F. ) ;
#363 = VERTEX_POINT ( 'NONE', #5799 ) ;
#364 = VERTEX_POINT ( 'NONE', #10563 ) ;
#365 = EDGE_LOOP ( 'NONE', ( #4634, #310, #4264, #5091 ) ) ;
#366 = DIRECTION ( 'NONE',  ( -1.000000000000000000, 1.006188713385347367E-17, 3.844790828812615713E-17 ) ) ;
#367 = ADVANCED_FACE ( 'NONE', ( #4841 ), #6716, .F. ) ;
#368 = EDGE_CURVE ( 'NONE', #6626, #7571, #10720, .T. ) ;
#369 = DIRECTION ( 'NONE',  ( 1.000000000000000000, 5.916456789157575403E-31, -1.577021341797098793E-16 ) ) ;
#370 = EDGE_LOOP ( 'NONE', ( #12481, #7079, #9486, #1457, #9621, #6938, #4666 ) ) ;
#371 = CARTESIAN_POINT ( 'NONE',  ( 33.00000000000001421, 81.84122341717352356, -52.68198508464163154 ) ) ;
#372 = EDGE_LOOP ( 'NONE', ( #7956, #11236, #11285, #3395 ) ) ;
#373 = CARTESIAN_POINT ( 'NONE',  ( -0.6920835326022437561, -4.454600218803894229, -3.597382984111584303 ) ) ;
#374 = DIRECTION ( 'NONE',  ( -1.000000000000000000, 1.010728034814421376E-30, 1.090846720500930387E-30 ) ) ;
#375 = EDGE_CURVE ( 'NONE', #9475, #4011, #6203, .T. ) ;
#376 = CARTESIAN_POINT ( 'NONE',  ( 3.455068668934421883, -2.624017327439090774, -3.316620875263736057 ) ) ;
#377 = ADVANCED_FACE ( 'NONE', ( #8824 ), #11672, .F. ) ;
#378 = DIRECTION ( 'NONE',  ( -1.000000000000000000, -1.031065855027150586E-29, 2.218671295934095703E-30 ) ) ;
#379 = ORIENTED_EDGE ( 'NONE', *, *, #2110, .T. ) ;
#380 = EDGE_LOOP ( 'NONE', ( #7389, #11762, #9800, #764, #11312 ) ) ;
#381 = CARTESIAN_POINT ( 'NONE',  ( 34.00000000000000000, 2.210487472460973191E-16, -1.610000000000017417 ) ) ;
#382 = EDGE_CURVE ( 'NONE', #5244, #271, #8885, .T. ) ;
#383 = CIRCLE ( 'NONE', #8612, 3.999999999999997335 ) ;
#384 = PRESENTATION_STYLE_ASSIGNMENT (( #9321 ) ) ;
#385 = LINE ( 'NONE', #10217, #5971 ) ;
#386 = DIRECTION ( 'NONE',  ( 0.000000000000000000, -0.9909497617679332571, -0.1342332658176667859 ) ) ;
#387 = AXIS2_PLACEMENT_3D ( 'NONE', #558, #4558, #8470 ) ;
#388 = AXIS2_PLACEMENT_3D ( 'NONE', #12442, #3619, #6573 ) ;
#389 = CARTESIAN_POINT ( 'NONE',  ( 4.000000000000001776, -2.471525695159820124, -3.686886880705778413 ) ) ;
#390 = CARTESIAN_POINT ( 'NONE',  ( 0.000000000000000000, 6.718789039999997215, -3.101269713516732196 ) ) ;
#391 = STYLED_ITEM ( 'NONE', ( #419 ), #1696 ) ;
#392 = CARTESIAN_POINT ( 'NONE',  ( 11.00000000000003730, -19.99999999999999645, 12.00000000000003553 ) ) ;
#393 = ORIENTED_EDGE ( 'NONE', *, *, #2969, .F. ) ;
#394 = CARTESIAN_POINT ( 'NONE',  ( 4.175002511812154538, 2.208363329454888113, -3.469254087858248514 ) ) ;
#395 = CARTESIAN_POINT ( 'NONE',  ( 14.00000000000000000, 12.99999999999999822, -4.000000000000000000 ) ) ;
#396 = VECTOR ( 'NONE', #12270, 999.9999999999998863 ) ;
#397 = AXIS2_PLACEMENT_3D ( 'NONE', #3147, #6392, #6023 ) ;
#398 = VECTOR ( 'NONE', #6706, 1000.000000000000000 ) ;
#399 = ORIENTED_EDGE ( 'NONE', *, *, #1607, .F. ) ;
#400 = FACE_OUTER_BOUND ( 'NONE', #10400, .T. ) ;
#401 = DIRECTION ( 'NONE',  ( -1.000000000000000000, 1.010728034814421376E-30, 1.090846720500930387E-30 ) ) ;
#402 =( BOUNDED_SURFACE ( )  B_SPLINE_SURFACE ( 3, 2, ( 
 ( #8030, #7078, #2118 ),
 ( #6038, #5976, #6104 ),
 ( #8162, #6231, #12104 ),
 ( #10929, #10141, #1331 ),
 ( #1144, #2182, #12042 ),
 ( #5263, #5013, #10861 ) ),
 .UNSPECIFIED., .F., .F., .F. ) 
 B_SPLINE_SURFACE_WITH_KNOTS ( ( 4, 2, 4 ),
 ( 3, 3 ),
 ( 0.02032853247518126918, 0.02278863295364821906, 0.02524873343211516893 ),
 ( 0.000000000000000000, 1.000000000000000000 ),
 .UNSPECIFIED. ) 
 GEOMETRIC_REPRESENTATION_ITEM ( )  RATIONAL_B_SPLINE_SURFACE ( (
 ( 1.000000000000000000, 0.8047781615896838492, 1.000000000000000000),
 ( 1.000000000000000000, 0.8123767586288899167, 1.000000000000000000),
 ( 1.000000000000000000, 0.8190662415564865517, 1.000000000000000000),
 ( 1.000000000000000000, 0.8192361015668555568, 1.000000000000000000),
 ( 1.000000000000000000, 0.8126135807104249986, 1.000000000000000000),
 ( 1.000000000000000000, 0.8047712338318584457, 1.000000000000000000) ) ) 
 REPRESENTATION_ITEM ( '' )  SURFACE ( )  );
#403 = FACE_OUTER_BOUND ( 'NONE', #8812, .T. ) ;
#404 = CARTESIAN_POINT ( 'NONE',  ( 1.734723475976807094E-14, -3.469446951953614189E-15, -4.000000000000010658 ) ) ;
#405 = CIRCLE ( 'NONE', #4524, 2.800000000000003375 ) ;
#406 = VECTOR ( 'NONE', #8142, 1000.000000000000000 ) ;
#407 = DIRECTION ( 'NONE',  ( 0.000000000000000000, 1.000000000000000000, 0.000000000000000000 ) ) ;
#408 = CARTESIAN_POINT ( 'NONE',  ( 2.500000000000035527, -3.163285252166775924E-15, -4.974600000000009459 ) ) ;
#409 = APPLICATION_CONTEXT ( 'automotive_design' ) ;
#410 = ORIENTED_EDGE ( 'NONE', *, *, #7161, .T. ) ;
#411 = DIRECTION ( 'NONE',  ( 1.000000000000000000, -0.000000000000000000, -0.000000000000000000 ) ) ;
#412 = VERTEX_POINT ( 'NONE', #4779 ) ;
#413 = ORIENTED_EDGE ( 'NONE', *, *, #5103, .T. ) ;
#414 = EDGE_CURVE ( 'NONE', #9874, #11663, #6658, .T. ) ;
#415 = ADVANCED_FACE ( 'NONE', ( #12584 ), #4715, .F. ) ;
#416 = VECTOR ( 'NONE', #1989, 1000.000000000000114 ) ;
#417 = EDGE_LOOP ( 'NONE', ( #3681, #5632, #1581, #10908 ) ) ;
#418 = CIRCLE ( 'NONE', #12362, 2.800000000000002931 ) ;
#419 = PRESENTATION_STYLE_ASSIGNMENT (( #10127 ) ) ;
#420 = FACE_OUTER_BOUND ( 'NONE', #1460, .T. ) ;
#421 = CARTESIAN_POINT ( 'NONE',  ( 40.00000000000000711, 18.52447679111068268, -16.77732469694377926 ) ) ;
#422 = CARTESIAN_POINT ( 'NONE',  ( 19.99999999999999645, 0.000000000000000000, 0.000000000000000000 ) ) ;
#423 = CARTESIAN_POINT ( 'NONE',  ( 33.00000000000000711, 58.55522666905708462, -36.77936687539386185 ) ) ;
#424 = ORIENTED_EDGE ( 'NONE', *, *, #89, .T. ) ;
#425 = DIRECTION ( 'NONE',  ( 0.000000000000000000, -0.9554649393887557629, 0.2951046417778634412 ) ) ;
#426 = DIRECTION ( 'NONE',  ( 1.000000000000000000, -6.162975822039154730E-33, -4.563833282352349791E-17 ) ) ;
#427 = ORIENTED_EDGE ( 'NONE', *, *, #12083, .T. ) ;
#428 = ORIENTED_EDGE ( 'NONE', *, *, #736, .F. ) ;
#429 = ORIENTED_EDGE ( 'NONE', *, *, #2954, .F. ) ;
#430 = ORIENTED_EDGE ( 'NONE', *, *, #2792, .F. ) ;
#431 = DIRECTION ( 'NONE',  ( 0.000000000000000000, -0.2951046417778627751, -0.9554649393887560960 ) ) ;
#432 = ADVANCED_FACE ( 'NONE', ( #10629 ), #7678, .T. ) ;
#433 = SURFACE_SIDE_STYLE ('',( #11389 ) ) ;
#434 = PRODUCT_RELATED_PRODUCT_CATEGORY ( 'part', '', ( #2709 ) ) ;
#435 = ORIENTED_EDGE ( 'NONE', *, *, #843, .T. ) ;
#436 = CARTESIAN_POINT ( 'NONE',  ( -11.83215956619923226, 30.00000000000000000, -4.336808689942017736E-16 ) ) ;
#437 = ORIENTED_EDGE ( 'NONE', *, *, #10607, .F. ) ;
#438 = DIRECTION ( 'NONE',  ( 0.000000000000000000, -1.530455820933490821E-32, 1.000000000000000000 ) ) ;
#439 = DIRECTION ( 'NONE',  ( -1.000000000000000000, 0.000000000000000000, 0.000000000000000000 ) ) ;
#440 = DIRECTION ( 'NONE',  ( -1.000000000000000000, 1.010728034814421376E-30, 1.090846720500930387E-30 ) ) ;
#441 = DIRECTION ( 'NONE',  ( 1.000000000000000000, 0.000000000000000000, 0.000000000000000000 ) ) ;
#442 = EDGE_LOOP ( 'NONE', ( #11196, #8941, #10732, #3335 ) ) ;
#443 = CIRCLE ( 'NONE', #3735, 7.400000000000009237 ) ;
#444 = VERTEX_POINT ( 'NONE', #9653 ) ;
#445 = EDGE_CURVE ( 'NONE', #3047, #865, #7801, .T. ) ;
#446 = DIRECTION ( 'NONE',  ( 0.000000000000000000, 0.000000000000000000, 1.000000000000000000 ) ) ;
#447 =( NAMED_UNIT ( * ) PLANE_ANGLE_UNIT ( ) SI_UNIT ( $, .RADIAN. ) );
#448 = EDGE_CURVE ( 'NONE', #992, #6318, #11736, .T. ) ;
#449 = CARTESIAN_POINT ( 'NONE',  ( -3.999999999999994671, 0.000000000000000000, 8.673617379884035472E-15 ) ) ;
#450 = EDGE_CURVE ( 'NONE', #4892, #8146, #2866, .T. ) ;
#451 = CARTESIAN_POINT ( 'NONE',  ( 33.00000000000001421, 81.84122341717352356, -27.68198508464163510 ) ) ;
#452 = AXIS2_PLACEMENT_3D ( 'NONE', #4456, #11224, #9272 ) ;
#453 = DIRECTION ( 'NONE',  ( -1.000000000000000000, -1.081682119347366444E-16, 5.551115123125780237E-17 ) ) ;
#454 = EDGE_CURVE ( 'NONE', #1459, #9808, #2931, .T. ) ;
#455 = CARTESIAN_POINT ( 'NONE',  ( -45.00000000000012079, -19.99999999999999645, 2.000000000000007994 ) ) ;
#456 = LINE ( 'NONE', #2532, #2255 ) ;
#457 = ORIENTED_EDGE ( 'NONE', *, *, #9263, .T. ) ;
#458 = CARTESIAN_POINT ( 'NONE',  ( 4.235886605889391809, 2.417314728048526984, -3.751161874094022686 ) ) ;
#459 = CARTESIAN_POINT ( 'NONE',  ( 19.99999999999997868, -3.055252325922143797, -5.825248672282175910 ) ) ;
#460 = VECTOR ( 'NONE', #2524, 1000.000000000000000 ) ;
#461 =( NAMED_UNIT ( * ) SI_UNIT ( $, .STERADIAN. ) SOLID_ANGLE_UNIT ( ) );
#462 = ADVANCED_FACE ( 'NONE', ( #3998 ), #9588, .T. ) ;
#463 = EDGE_LOOP ( 'NONE', ( #110, #9977 ) ) ;
#464 = DIRECTION ( 'NONE',  ( 0.000000000000000000, 0.000000000000000000, -1.000000000000000000 ) ) ;
#465 = CARTESIAN_POINT ( 'NONE',  ( 19.99999999999999645, 0.000000000000000000, 0.000000000000000000 ) ) ;
#466 = DIRECTION ( 'NONE',  ( -1.380506584136768733E-30, 0.4338837391175524583, 0.9009688679024216995 ) ) ;
#467 = DIRECTION ( 'NONE',  ( 0.000000000000000000, 0.000000000000000000, -1.000000000000000000 ) ) ;
#468 = AXIS2_PLACEMENT_3D ( 'NONE', #1619, #6323, #10228 ) ;
#469 = DIRECTION ( 'NONE',  ( -1.000000000000000000, 0.000000000000000000, 1.301042606982605074E-16 ) ) ;
#470 = CIRCLE ( 'NONE', #9303, 2.800000000000003819 ) ;
#471 = DIRECTION ( 'NONE',  ( 0.000000000000000000, 0.000000000000000000, -1.000000000000000000 ) ) ;
#472 = CARTESIAN_POINT ( 'NONE',  ( -17.00000000000000000, -30.00000000000000000, 3.000000000000030198 ) ) ;
#473 = ORIENTED_EDGE ( 'NONE', *, *, #1787, .F. ) ;
#474 = DIRECTION ( 'NONE',  ( 1.000000000000000000, 1.031065855027150586E-29, -2.218671295934095703E-30 ) ) ;
#475 = ORIENTED_EDGE ( 'NONE', *, *, #9984, .T. ) ;
#476 = CIRCLE ( 'NONE', #5414, 10.00000000000000178 ) ;
#477 = VERTEX_POINT ( 'NONE', #10690 ) ;
#478 = CONTEXT_DEPENDENT_SHAPE_REPRESENTATION ( #4117, #6890 ) ;
#479 = VERTEX_POINT ( 'NONE', #10750 ) ;
#480 = FILL_AREA_STYLE ('',( #5374 ) ) ;
#481 = EDGE_CURVE ( 'NONE', #1188, #12214, #2518, .T. ) ;
#482 = CARTESIAN_POINT ( 'NONE',  ( 0.000000000000000000, 0.6915992404090791634, -6.462096524400238629 ) ) ;
#483 = DIRECTION ( 'NONE',  ( -9.614242282381067365E-31, -0.08963930890344089242, 0.9959742939952382912 ) ) ;
#484 = CYLINDRICAL_SURFACE ( 'NONE', #199, 10.00000000000000000 ) ;
#485 = DIRECTION ( 'NONE',  ( -1.000000000000000000, 1.010728034814421376E-30, 1.090846720500930387E-30 ) ) ;
#486 = ORIENTED_EDGE ( 'NONE', *, *, #4954, .F. ) ;
#487 = CARTESIAN_POINT ( 'NONE',  ( 4.211140560182228043, -2.431303136016558231, -3.745885042887437510 ) ) ;
#488 = AXIS2_PLACEMENT_3D ( 'NONE', #8589, #5753, #5691 ) ;
#489 = FACE_BOUND ( 'NONE', #6630, .T. ) ;
#490 = VERTEX_POINT ( 'NONE', #12059 ) ;
#491 = ORIENTED_EDGE ( 'NONE', *, *, #11638, .F. ) ;
#492 = ORIENTED_EDGE ( 'NONE', *, *, #6966, .T. ) ;
#493 = ORIENTED_EDGE ( 'NONE', *, *, #2028, .F. ) ;
#494 = CIRCLE ( 'NONE', #6686, 3.500000000000003997 ) ;
#495 = LINE ( 'NONE', #10139, #8704 ) ;
#496 = PLANE ( 'NONE',  #10808 ) ;
#497 = ORIENTED_EDGE ( 'NONE', *, *, #10237, .F. ) ;
#498 = DIRECTION ( 'NONE',  ( -1.000000000000000000, 1.010728034814421376E-30, -1.140150527077241873E-30 ) ) ;
#499 = VERTEX_POINT ( 'NONE', #4254 ) ;
#500 = DIRECTION ( 'NONE',  ( 0.000000000000000000, -0.9554649393887557629, 0.2951046417778634412 ) ) ;
#501 = LINE ( 'NONE', #5270, #9745 ) ;
#502 = VECTOR ( 'NONE', #1677, 1000.000000000000000 ) ;
#503 = CIRCLE ( 'NONE', #12641, 2.500000000000003553 ) ;
#504 = ADVANCED_FACE ( 'NONE', ( #4128 ), #325, .T. ) ;
#505 = CARTESIAN_POINT ( 'NONE',  ( 20.00000000000000000, 21.12780530657007461, -5.807015647486883481 ) ) ;
#506 = ADVANCED_FACE ( 'NONE', ( #6248 ), #8873, .T. ) ;
#507 = EDGE_CURVE ( 'NONE', #8913, #7082, #5814, .T. ) ;
#508 = LINE ( 'NONE', #572, #8236 ) ;
#509 = VERTEX_POINT ( 'NONE', #8950 ) ;
#510 = ORIENTED_EDGE ( 'NONE', *, *, #6287, .F. ) ;
#511 = CARTESIAN_POINT ( 'NONE',  ( 40.00000000000000711, 15.24625277455639250, -6.248133273622505257 ) ) ;
#512 = CIRCLE ( 'NONE', #11620, 6.499000000000008548 ) ;
#513 = ADVANCED_FACE ( 'NONE', ( #2068 ), #7979, .T. ) ;
#514 = CIRCLE ( 'NONE', #2164, 2.800000000000003375 ) ;
#515 = FACE_OUTER_BOUND ( 'NONE', #12425, .T. ) ;
#516 = CARTESIAN_POINT ( 'NONE',  ( 19.99999999999999645, 1.395418990828201533, 6.428133065596412621 ) ) ;
#517 = PRODUCT_DEFINITION_SHAPE ( 'NONE', 'NONE',  #7290 ) ;
#518 = CARTESIAN_POINT ( 'NONE',  ( 4.000000000000001776, -0.8732470631450258702, -3.223155494240763197 ) ) ;
#519 = CYLINDRICAL_SURFACE ( 'NONE', #97, 6.499000000000010324 ) ;
#520 = AXIS2_PLACEMENT_3D ( 'NONE', #4632, #11202, #6301 ) ;
#521 = AXIS2_PLACEMENT_3D ( 'NONE', #8664, #3774, #5821 ) ;
#522 = CARTESIAN_POINT ( 'NONE',  ( -18.00000000000002842, -30.00000000000000000, 4.336808689942017736E-16 ) ) ;
#523 = ORIENTED_EDGE ( 'NONE', *, *, #7970, .F. ) ;
#524 = CARTESIAN_POINT ( 'NONE',  ( 1.287237434361733213, 3.875615274277073308, -3.430618716626818276 ) ) ;
#525 = CYLINDRICAL_SURFACE ( 'NONE', #241, 6.499000000000010324 ) ;
#526 = FILL_AREA_STYLE ('',( #12323 ) ) ;
#527 = EDGE_CURVE ( 'NONE', #837, #2437, #10330, .T. ) ;
#528 = DIRECTION ( 'NONE',  ( -1.000000000000000000, 1.010728034814421376E-30, 1.090846720500930387E-30 ) ) ;
#529 = VERTEX_POINT ( 'NONE', #2134 ) ;
#530 = CIRCLE ( 'NONE', #8546, 2.800000000000003819 ) ;
#531 = LINE ( 'NONE', #9277, #10738 ) ;
#532 = ADVANCED_FACE ( 'NONE', ( #11863 ), #11017, .F. ) ;
#533 = CARTESIAN_POINT ( 'NONE',  ( 19.99999999999999645, -5.682309657208315379, -3.313524683562055984 ) ) ;
#534 = CARTESIAN_POINT ( 'NONE',  ( 11.00000000000003020, 30.00000000000000000, 25.00000000000007105 ) ) ;
#535 = DIRECTION ( 'NONE',  ( -0.000000000000000000, -1.000000000000000000, -0.000000000000000000 ) ) ;
#536 = FACE_OUTER_BOUND ( 'NONE', #5367, .T. ) ;
#537 = EDGE_CURVE ( 'NONE', #41, #2105, #8074, .T. ) ;
#538 = CARTESIAN_POINT ( 'NONE',  ( -15.00000000000000000, 3.123110065765668157E-30, 22.15000000000006608 ) ) ;
#539 = ADVANCED_FACE ( 'NONE', ( #7031 ), #4318, .F. ) ;
#540 = LINE ( 'NONE', #408, #11927 ) ;
#541 = AXIS2_PLACEMENT_3D ( 'NONE', #8358, #12429, #3605 ) ;
#542 = CIRCLE ( 'NONE', #1350, 2.800000000000002931 ) ;
#543 = FACE_OUTER_BOUND ( 'NONE', #7089, .T. ) ;
#544 = ORIENTED_EDGE ( 'NONE', *, *, #9595, .F. ) ;
#545 = ORIENTED_EDGE ( 'NONE', *, *, #8383, .T. ) ;
#546 = ORIENTED_EDGE ( 'NONE', *, *, #11077, .T. ) ;
#547 = DIRECTION ( 'NONE',  ( 0.000000000000000000, 0.9909497617679351444, -0.1342332658176521309 ) ) ;
#548 = CARTESIAN_POINT ( 'NONE',  ( -15.00000000000003375, 19.99999999999998934, 12.00000000000002842 ) ) ;
#549 = FACE_OUTER_BOUND ( 'NONE', #3644, .T. ) ;
#550 = AXIS2_PLACEMENT_3D ( 'NONE', #4921, #8783, #1827 ) ;
#551 = CARTESIAN_POINT ( 'NONE',  ( 19.99999999999999645, 0.000000000000000000, 0.000000000000000000 ) ) ;
#552 = ORIENTED_EDGE ( 'NONE', *, *, #4771, .F. ) ;
#553 = VECTOR ( 'NONE', #2820, 1000.000000000000114 ) ;
#554 = DIRECTION ( 'NONE',  ( 1.000000000000000000, -6.162975822039154730E-33, -4.563833282352349791E-17 ) ) ;
#555 = CARTESIAN_POINT ( 'NONE',  ( 11.00000000000003020, -30.00000000000000000, 25.00000000000007105 ) ) ;
#556 = ORIENTED_EDGE ( 'NONE', *, *, #9689, .T. ) ;
#557 = ORIENTED_EDGE ( 'NONE', *, *, #3842, .T. ) ;
#558 = CARTESIAN_POINT ( 'NONE',  ( 2.000000000000001776, 1.773042676681338303, 0.000000000000000000 ) ) ;
#559 = ORIENTED_EDGE ( 'NONE', *, *, #8524, .T. ) ;
#560 = AXIS2_PLACEMENT_3D ( 'NONE', #7660, #1672, #10548 ) ;
#561 = VERTEX_POINT ( 'NONE', #3052 ) ;
#562 = VECTOR ( 'NONE', #12140, 999.9999999999998863 ) ;
#563 = VECTOR ( 'NONE', #1495, 1000.000000000000227 ) ;
#564 = EDGE_CURVE ( 'NONE', #7155, #8095, #3349, .T. ) ;
#565 = ORIENTED_EDGE ( 'NONE', *, *, #1103, .T. ) ;
#566 = FACE_OUTER_BOUND ( 'NONE', #2032, .T. ) ;
#567 = CARTESIAN_POINT ( 'NONE',  ( 40.00000000000000000, 39.49790820824818383, -24.06186359251417883 ) ) ;
#568 = VERTEX_POINT ( 'NONE', #6186 ) ;
#569 = CARTESIAN_POINT ( 'NONE',  ( 0.000000000000000000, 0.000000000000000000, 3.299999999999999822 ) ) ;
#570 = CARTESIAN_POINT ( 'NONE',  ( 40.00000000000000711, 19.99999999999999645, -14.14999999999999147 ) ) ;
#571 = DIRECTION ( 'NONE',  ( 0.000000000000000000, 1.530455820933490821E-32, -1.000000000000000000 ) ) ;
#572 = CARTESIAN_POINT ( 'NONE',  ( 11.00000000000003020, 30.00000000000000000, 5.000000000000004441 ) ) ;
#573 = EDGE_LOOP ( 'NONE', ( #4853, #5435, #11535, #9853, #12243 ) ) ;
#574 = VERTEX_POINT ( 'NONE', #5990 ) ;
#575 = DIRECTION ( 'NONE',  ( 1.238279320584846685E-16, -0.9554649393887560960, 0.2951046417778627751 ) ) ;
#576 = EDGE_CURVE ( 'NONE', #499, #3763, #3136, .T. ) ;
#577 = DIRECTION ( 'NONE',  ( -1.000000000000000000, -1.081682119347366197E-16, 6.938893903907228378E-17 ) ) ;
#578 = EDGE_CURVE ( 'NONE', #7319, #12298, #9904, .T. ) ;
#579 = DIRECTION ( 'NONE',  ( -1.000000000000000000, -1.031065855027150586E-29, 2.218671295934095703E-30 ) ) ;
#580 = CYLINDRICAL_SURFACE ( 'NONE', #12033, 2.149999999999992362 ) ;
#581 = CARTESIAN_POINT ( 'NONE',  ( 27.00000000000001421, 39.34792583643766761, -17.06347054209568270 ) ) ;
#582 = ORIENTED_EDGE ( 'NONE', *, *, #11922, .T. ) ;
#583 = CIRCLE ( 'NONE', #10028, 2.800000000000003819 ) ;
#584 = CARTESIAN_POINT ( 'NONE',  ( 19.99999999999999645, 0.000000000000000000, 0.000000000000000000 ) ) ;
#585 = CARTESIAN_POINT ( 'NONE',  ( 19.99999999999999645, 7.358375340956981425, 0.7837807994561900582 ) ) ;
#586 = DIRECTION ( 'NONE',  ( -1.000000000000000000, 1.010728034814421376E-30, 1.090846720500930387E-30 ) ) ;
#587 = EDGE_LOOP ( 'NONE', ( #5195, #2640, #8200, #5319 ) ) ;
#588 = CARTESIAN_POINT ( 'NONE',  ( 4.211140560182228043, -2.431303136016558231, -3.745885042887437510 ) ) ;
#589 = DIRECTION ( 'NONE',  ( 1.232595164407829545E-30, -0.9510565162951502005, -0.3090169943749582204 ) ) ;
#590 = VECTOR ( 'NONE', #4280, 1000.000000000000000 ) ;
#591 = CARTESIAN_POINT ( 'NONE',  ( 19.99999999999997868, -7.399010254356644722, -0.1210258481700032807 ) ) ;
#592 = CARTESIAN_POINT ( 'NONE',  ( 9.999999999999980460, -4.707829255731252438, 5.709320773864527965 ) ) ;
#593 = DIRECTION ( 'NONE',  ( -1.000000000000000000, 1.010728034814421376E-30, 1.090846720500930387E-30 ) ) ;
#594 = DIRECTION ( 'NONE',  ( -1.000000000000000000, 1.010728034814421376E-30, 1.090846720500930387E-30 ) ) ;
#595 = DIRECTION ( 'NONE',  ( 0.8191520442889902442, 1.003171929053522775E-16, -0.5735764363510482688 ) ) ;
#596 = CIRCLE ( 'NONE', #5947, 6.499000000000006771 ) ;
#597 = CIRCLE ( 'NONE', #1831, 24.99999999999998934 ) ;
#598 = COLOUR_RGB ( '', 0.40784314, 0.44705882, 0.49803922) ;
#599 = CARTESIAN_POINT ( 'NONE',  ( -4.211140560182210280, 2.431303136016527144, -3.745885042887430405 ) ) ;
#600 = ORIENTED_EDGE ( 'NONE', *, *, #3946, .T. ) ;
#601 = CIRCLE ( 'NONE', #2631, 2.800000000000003819 ) ;
#602 = ORIENTED_EDGE ( 'NONE', *, *, #3672, .F. ) ;
#603 = EDGE_CURVE ( 'NONE', #9871, #1141, #5181, .T. ) ;
#604 = ORIENTED_EDGE ( 'NONE', *, *, #7620, .T. ) ;
#605 = CARTESIAN_POINT ( 'NONE',  ( 0.000000000000000000, 0.000000000000000000, 0.000000000000000000 ) ) ;
#606 = ADVANCED_FACE ( 'NONE', ( #5163 ), #9078, .F. ) ;
#607 = CONICAL_SURFACE ( 'NONE', #3311, 1.610000000000000098, 0.7853981633974652654 ) ;
#608 = LINE ( 'NONE', #7632, #1578 ) ;
#609 = DIRECTION ( 'NONE',  ( 1.000000000000000000, 5.916456789157575403E-31, -1.577021341797098793E-16 ) ) ;
#610 = VECTOR ( 'NONE', #8698, 1000.000000000000000 ) ;
#611 = AXIS2_PLACEMENT_3D ( 'NONE', #6625, #6815, #10596 ) ;
#612 = CARTESIAN_POINT ( 'NONE',  ( 9.999999999999998224, 6.718789040000002544, -3.101269713516732196 ) ) ;
#613 = ORIENTED_EDGE ( 'NONE', *, *, #6988, .F. ) ;
#614 = CARTESIAN_POINT ( 'NONE',  ( 20.00000000000000000, 11.34118543499637077, -24.03007857557328464 ) ) ;
#615 = ADVANCED_FACE ( 'NONE', ( #7162 ), #11080, .F. ) ;
#616 = CARTESIAN_POINT ( 'NONE',  ( 20.00000000000000355, 18.52447679111067913, -16.77732469694377926 ) ) ;
#617 = ORIENTED_EDGE ( 'NONE', *, *, #7288, .T. ) ;
#618 = ORIENTED_EDGE ( 'NONE', *, *, #11395, .T. ) ;
#619 = PLANE ( 'NONE',  #7619 ) ;
#620 = ORIENTED_EDGE ( 'NONE', *, *, #4486, .F. ) ;
#621 = CIRCLE ( 'NONE', #7816, 9.999999999999998224 ) ;
#622 = EDGE_LOOP ( 'NONE', ( #3676, #3144, #3031 ) ) ;
#623 = CIRCLE ( 'NONE', #8615, 4.000000000000001776 ) ;
#624 = TOROIDAL_SURFACE ( 'NONE', #7821, 3.299999999999999822, 0.2000000000000000111 ) ;
#625 = DIRECTION ( 'NONE',  ( -1.848892746611746419E-31, -1.000000000000000000, 3.250006781153460502E-32 ) ) ;
#626 = EDGE_LOOP ( 'NONE', ( #2632, #9006, #9669, #2831 ) ) ;
#627 = CARTESIAN_POINT ( 'NONE',  ( 0.000000000000000000, -5.774092856145738750, 2.982759240804853107 ) ) ;
#628 = DIRECTION ( 'NONE',  ( -1.000000000000000000, 0.000000000000000000, 1.159061634649218351E-16 ) ) ;
#629 = ORIENTED_EDGE ( 'NONE', *, *, #3742, .F. ) ;
#630 = DIRECTION ( 'NONE',  ( 2.218671295934092637E-31, -0.8345732537213078617, 0.5508969814520944253 ) ) ;
#631 = LINE ( 'NONE', #12621, #6264 ) ;
#632 = COLOUR_RGB ( '', 0.66274510, 0.83137255, 0.94901961) ;
#633 = TOROIDAL_SURFACE ( 'NONE', #12373, 4.999999999999997335, 4.000000000000000000 ) ;
#634 = CARTESIAN_POINT ( 'NONE',  ( 0.000000000000000000, -6.182645281642508372, 2.245659411033100294 ) ) ;
#635 = CARTESIAN_POINT ( 'NONE',  ( 0.000000000000000000, 0.000000000000000000, 0.000000000000000000 ) ) ;
#636 = EDGE_LOOP ( 'NONE', ( #8469, #3542, #10384, #4361 ) ) ;
#637 = ORIENTED_EDGE ( 'NONE', *, *, #11083, .T. ) ;
#638 = DIRECTION ( 'NONE',  ( 0.000000000000000000, 1.000000000000000000, 0.000000000000000000 ) ) ;
#639 =( GEOMETRIC_REPRESENTATION_CONTEXT ( 3 ) GLOBAL_UNCERTAINTY_ASSIGNED_CONTEXT ( ( #2646 ) ) GLOBAL_UNIT_ASSIGNED_CONTEXT ( ( #12452, #11860, #2199 ) ) REPRESENTATION_CONTEXT ( 'NONE', 'WORKASPACE' ) );
#640 = VERTEX_POINT ( 'NONE', #9383 ) ;
#641 = CARTESIAN_POINT ( 'NONE',  ( -4.211140560182210280, 2.431303136016527144, -3.745885042887430405 ) ) ;
#642 = CARTESIAN_POINT ( 'NONE',  ( 33.00000000000000000, 14.50364731389636397, -24.59751492040896892 ) ) ;
#643 = DIRECTION ( 'NONE',  ( 0.000000000000000000, 0.000000000000000000, -1.000000000000000000 ) ) ;
#644 = AXIS2_PLACEMENT_3D ( 'NONE', #4663, #8717, #5810 ) ;
#645 = CARTESIAN_POINT ( 'NONE',  ( 19.99999999999999645, 0.000000000000000000, 0.000000000000000000 ) ) ;
#646 = EDGE_CURVE ( 'NONE', #2961, #11067, #5786, .T. ) ;
#647 = ORIENTED_EDGE ( 'NONE', *, *, #2202, .T. ) ;
#648 = DIRECTION ( 'NONE',  ( -1.000000000000000000, 1.010728034814421376E-30, 1.090846720500930387E-30 ) ) ;
#649 = DIRECTION ( 'NONE',  ( 1.000000000000000000, -1.010728034814421376E-30, -1.090846720500930387E-30 ) ) ;
#650 = CARTESIAN_POINT ( 'NONE',  ( 19.99999999999997868, 6.359534927042319374, -1.339147681075104845 ) ) ;
#651 = ORIENTED_EDGE ( 'NONE', *, *, #537, .F. ) ;
#652 = DIRECTION ( 'NONE',  ( -1.000000000000000000, -5.916456789157575403E-31, 1.577021341797098793E-16 ) ) ;
#653 = CARTESIAN_POINT ( 'NONE',  ( -10.00000000000000178, 0.000000000000000000, 0.000000000000000000 ) ) ;
#654 = CARTESIAN_POINT ( 'NONE',  ( 19.99999999999997868, -3.055252325922143797, -5.825248672282175910 ) ) ;
#655 = CARTESIAN_POINT ( 'NONE',  ( 0.6920835326022525269, 4.454600218803853373, -3.597382984111599846 ) ) ;
#656 = CARTESIAN_POINT ( 'NONE',  ( 19.99999999999999645, -6.453973581750240385, 0.7636923504068631186 ) ) ;
#657 = CARTESIAN_POINT ( 'NONE',  ( 19.99999999999999645, -4.907279493584704610, -4.380262188593404105 ) ) ;
#658 = EDGE_CURVE ( 'NONE', #5057, #3716, #851, .T. ) ;
#659 = AXIS2_PLACEMENT_3D ( 'NONE', #128, #5987, #1992 ) ;
#660 = ADVANCED_FACE ( 'NONE', ( #5603, #1675 ), #8249, .T. ) ;
#661 = LINE ( 'NONE', #3823, #6580 ) ;
#662 = UNCERTAINTY_MEASURE_WITH_UNIT (LENGTH_MEASURE( 1.000000000000000082E-05 ), #8919, 'distance_accuracy_value', 'NONE');
#663 = EDGE_CURVE ( 'NONE', #8684, #9579, #239, .T. ) ;
#664 = LINE ( 'NONE', #7811, #3937 ) ;
#665 = ORIENTED_EDGE ( 'NONE', *, *, #1472, .F. ) ;
#666 = EDGE_CURVE ( 'NONE', #10338, #2092, #3944, .T. ) ;
#667 = ORIENTED_EDGE ( 'NONE', *, *, #12742, .T. ) ;
#668 = ORIENTED_EDGE ( 'NONE', *, *, #10011, .T. ) ;
#669 = AXIS2_PLACEMENT_3D ( 'NONE', #3194, #5107, #7170 ) ;
#670 = DIRECTION ( 'NONE',  ( 0.000000000000000000, 0.000000000000000000, 1.000000000000000000 ) ) ;
#671 = CIRCLE ( 'NONE', #10117, 2.149999999999985256 ) ;
#672 = DIRECTION ( 'NONE',  ( 0.000000000000000000, 0.000000000000000000, 1.000000000000000000 ) ) ;
#673 = CARTESIAN_POINT ( 'NONE',  ( 11.00000000000003020, 30.00000000000000000, 25.00000000000007105 ) ) ;
#674 = LINE ( 'NONE', #10390, #9169 ) ;
#675 = ORIENTED_EDGE ( 'NONE', *, *, #4358, .T. ) ;
#676 = PLANE ( 'NONE',  #3004 ) ;
#677 = DIRECTION ( 'NONE',  ( -1.000000000000000000, 1.010728034814421376E-30, 1.090846720500930387E-30 ) ) ;
#678 = ORIENTED_EDGE ( 'NONE', *, *, #5317, .T. ) ;
#679 = VECTOR ( 'NONE', #1002, 1000.000000000000000 ) ;
#680 = ORIENTED_EDGE ( 'NONE', *, *, #6194, .F. ) ;
#681 = LINE ( 'NONE', #4618, #8814 ) ;
#682 = ORIENTED_EDGE ( 'NONE', *, *, #2205, .T. ) ;
#683 = ORIENTED_EDGE ( 'NONE', *, *, #10659, .F. ) ;
#684 = FACE_OUTER_BOUND ( 'NONE', #282, .T. ) ;
#685 = ORIENTED_EDGE ( 'NONE', *, *, #8630, .F. ) ;
#686 = CARTESIAN_POINT ( 'NONE',  ( 0.000000000000000000, 0.000000000000000000, 0.000000000000000000 ) ) ;
#687 = EDGE_CURVE ( 'NONE', #1778, #3832, #1883, .T. ) ;
#688 = FACE_OUTER_BOUND ( 'NONE', #7012, .T. ) ;
#689 = ORIENTED_EDGE ( 'NONE', *, *, #4230, .F. ) ;
#690 = AXIS2_PLACEMENT_3D ( 'NONE', #10582, #5815, #11751 ) ;
#691 = FACE_OUTER_BOUND ( 'NONE', #7606, .T. ) ;
#692 = CARTESIAN_POINT ( 'NONE',  ( 33.61000000000001364, 2.449293598294697047E-16, -2.000000000000000888 ) ) ;
#693 = CARTESIAN_POINT ( 'NONE',  ( 2.100000000000035172, -3.469446951953614189E-15, -5.000000000000011546 ) ) ;
#694 = UNCERTAINTY_MEASURE_WITH_UNIT (LENGTH_MEASURE( 1.000000000000000082E-05 ), #1092, 'distance_accuracy_value', 'NONE');
#695 = EDGE_CURVE ( 'NONE', #11780, #5322, #2587, .T. ) ;
#696 = EDGE_CURVE ( 'NONE', #7580, #4994, #1265, .T. ) ;
#697 = EDGE_LOOP ( 'NONE', ( #7888, #5340, #1354, #8282 ) ) ;
#698 = ORIENTED_EDGE ( 'NONE', *, *, #11571, .F. ) ;
#699 = DIRECTION ( 'NONE',  ( 1.000000000000000000, 1.081682119347366197E-16, -6.938893903907228378E-17 ) ) ;
#700 = CARTESIAN_POINT ( 'NONE',  ( 13.00000000000000355, 20.00000000000002132, -12.00000000000009770 ) ) ;
#701 = VERTEX_POINT ( 'NONE', #1411 ) ;
#702 = CARTESIAN_POINT ( 'NONE',  ( 27.00000000000000355, 29.58047730022061472, -27.90351864933187898 ) ) ;
#703 = CIRCLE ( 'NONE', #10980, 3.000000000000005773 ) ;
#704 = CARTESIAN_POINT ( 'NONE',  ( 19.99999999999999645, 0.000000000000000000, 0.000000000000000000 ) ) ;
#705 = CARTESIAN_POINT ( 'NONE',  ( 13.63191942669736889, 12.50000000000000000, 3.758770483143645702 ) ) ;
#706 = EDGE_CURVE ( 'NONE', #2862, #4036, #4572, .T. ) ;
#707 = LINE ( 'NONE', #10430, #5346 ) ;
#708 = EDGE_LOOP ( 'NONE', ( #5484, #4858 ) ) ;
#709 = DIRECTION ( 'NONE',  ( -1.000000000000000000, 1.010728034814421376E-30, 1.090846720500930387E-30 ) ) ;
#710 = CIRCLE ( 'NONE', #1557, 12.00000000000000000 ) ;
#711 = VERTEX_POINT ( 'NONE', #7351 ) ;
#712 = AXIS2_PLACEMENT_3D ( 'NONE', #10541, #1663, #1727 ) ;
#713 = CARTESIAN_POINT ( 'NONE',  ( 40.00000000000000711, 11.34118543499637255, -24.03007857557328464 ) ) ;
#714 = EDGE_CURVE ( 'NONE', #1261, #7962, #3815, .T. ) ;
#715 = EDGE_CURVE ( 'NONE', #3334, #12136, #930, .T. ) ;
#716 = CARTESIAN_POINT ( 'NONE',  ( 19.99999999999997868, 0.4528593230175830819, -7.386130139224213131 ) ) ;
#717 = CARTESIAN_POINT ( 'NONE',  ( 0.000000000000000000, 5.200656487704347519, -5.264330166022919144 ) ) ;
#718 = DIRECTION ( 'NONE',  ( 0.000000000000000000, -1.530455820933490821E-32, 1.000000000000000000 ) ) ;
#720 = CARTESIAN_POINT ( 'NONE',  ( 0.3198814748697545451, 4.434118497892176158, -0.3507732604232445817 ) ) ;
#719 = CIRCLE ( 'NONE', #8935, 7.400000000000009237 ) ;
#721 = CARTESIAN_POINT ( 'NONE',  ( 14.00000000000000000, -12.99999999999999822, 0.000000000000000000 ) ) ;
#722 = DIRECTION ( 'NONE',  ( -0.000000000000000000, 1.000000000000000000, 0.000000000000000000 ) ) ;
#723 = CARTESIAN_POINT ( 'NONE',  ( 0.000000000000000000, 6.544726022087268724, -0.6592800351836389794 ) ) ;
#724 = PRODUCT ( 'cover 2', 'cover 2', '', ( #8914 ) ) ;
#725 = CARTESIAN_POINT ( 'NONE',  ( 20.00000000000000000, 12.07894703944102766, -21.64141622710139146 ) ) ;
#726 = ADVANCED_FACE ( 'NONE', ( #8496 ), #11276, .T. ) ;
#727 = CARTESIAN_POINT ( 'NONE',  ( 14.00000000000000000, -13.00000000000000000, 0.000000000000000000 ) ) ;
#728 = ORIENTED_EDGE ( 'NONE', *, *, #9809, .F. ) ;
#729 = VECTOR ( 'NONE', #11677, 1000.000000000000000 ) ;
#730 = ORIENTED_EDGE ( 'NONE', *, *, #7700, .F. ) ;
#731 = ORIENTED_EDGE ( 'NONE', *, *, #143, .T. ) ;
#732 = ADVANCED_FACE ( 'NONE', ( #12312 ), #11410, .T. ) ;
#733 = LINE ( 'NONE', #12601, #6869 ) ;
#734 = DIRECTION ( 'NONE',  ( 1.000000000000000000, 5.916456789157575403E-31, -1.577021341797098793E-16 ) ) ;
#736 = EDGE_CURVE ( 'NONE', #1153, #9287, #7907, .T. ) ;
#735 = CYLINDRICAL_SURFACE ( 'NONE', #7583, 19.99999999999999645 ) ;
#737 = DIRECTION ( 'NONE',  ( -1.848892746611746419E-31, -1.000000000000000000, 3.250006781153460502E-32 ) ) ;
#738 = EDGE_LOOP ( 'NONE', ( #5945, #4675, #6555, #11845 ) ) ;
#739 = FACE_OUTER_BOUND ( 'NONE', #4229, .T. ) ;
#740 = CIRCLE ( 'NONE', #11855, 2.499999999999999556 ) ;
#741 = FACE_OUTER_BOUND ( 'NONE', #4025, .T. ) ;
#742 = VERTEX_POINT ( 'NONE', #12444 ) ;
#743 = ORIENTED_EDGE ( 'NONE', *, *, #7941, .T. ) ;
#744 = DIRECTION ( 'NONE',  ( 1.000000000000000000, 0.000000000000000000, 0.000000000000000000 ) ) ;
#745 = EDGE_LOOP ( 'NONE', ( #5637, #3870, #2752, #943 ) ) ;
#746 = ORIENTED_EDGE ( 'NONE', *, *, #10417, .F. ) ;
#747 = FACE_OUTER_BOUND ( 'NONE', #12689, .T. ) ;
#748 = EDGE_LOOP ( 'NONE', ( #2877, #7113, #11794, #1502 ) ) ;
#749 = VECTOR ( 'NONE', #6801, 1000.000000000000000 ) ;
#750 = DIRECTION ( 'NONE',  ( 0.000000000000000000, -1.000000000000000000, 0.000000000000000000 ) ) ;
#751 = AXIS2_PLACEMENT_3D ( 'NONE', #5443, #1637, #672 ) ;
#752 = CARTESIAN_POINT ( 'NONE',  ( 19.99999999999999645, -2.720702104307051172, 5.902099716170436494 ) ) ;
#753 = VERTEX_POINT ( 'NONE', #6513 ) ;
#754 = EDGE_CURVE ( 'NONE', #5455, #175, #6337, .T. ) ;
#755 = CARTESIAN_POINT ( 'NONE',  ( 0.000000000000000000, -2.720702104306971236, -5.902099716170491561 ) ) ;
#756 = CARTESIAN_POINT ( 'NONE',  ( 19.99999999999997868, 3.238809497145301197, -5.634457741540144227 ) ) ;
#757 = AXIS2_PLACEMENT_3D ( 'NONE', #9994, #4870, #4996 ) ;
#758 = EDGE_CURVE ( 'NONE', #3906, #5156, #7358, .T. ) ;
#759 = CIRCLE ( 'NONE', #7352, 6.499000000000009436 ) ;
#760 = ORIENTED_EDGE ( 'NONE', *, *, #8868, .F. ) ;
#761 = ORIENTED_EDGE ( 'NONE', *, *, #4308, .F. ) ;
#762 = CARTESIAN_POINT ( 'NONE',  ( 40.00000000000000711, 10.26855730552414059, -22.42000078613342851 ) ) ;
#763 = DIRECTION ( 'NONE',  ( 0.000000000000000000, 0.000000000000000000, 1.000000000000000000 ) ) ;
#764 = ORIENTED_EDGE ( 'NONE', *, *, #1551, .T. ) ;
#765 = CARTESIAN_POINT ( 'NONE',  ( 0.000000000000000000, 0.000000000000000000, 0.000000000000000000 ) ) ;
#766 = ADVANCED_FACE ( 'NONE', ( #4512, #5069, #893, #8688 ), #2728, .F. ) ;
#767 = CARTESIAN_POINT ( 'NONE',  ( 40.00000000000000711, 30.14235464176399404, -24.26236220746664785 ) ) ;
#768 = AXIS2_PLACEMENT_3D ( 'NONE', #5005, #48, #5840 ) ;
#769 = ADVANCED_FACE ( 'NONE', ( #3739 ), #9034, .T. ) ;
#770 = CARTESIAN_POINT ( 'NONE',  ( 0.000000000000000000, 0.000000000000000000, 0.000000000000000000 ) ) ;
#771 = DIRECTION ( 'NONE',  ( -0.000000000000000000, -1.000000000000000000, -0.000000000000000000 ) ) ;
#772 = EDGE_CURVE ( 'NONE', #5440, #1077, #5854, .T. ) ;
#773 = ORIENTED_EDGE ( 'NONE', *, *, #7954, .F. ) ;
#774 = CARTESIAN_POINT ( 'NONE',  ( 4.000000000000001776, 2.309401076758487381, -3.433295621305364254 ) ) ;
#775 = ORIENTED_EDGE ( 'NONE', *, *, #6278, .F. ) ;
#776 = DIRECTION ( 'NONE',  ( 4.606824426974261154E-31, 0.5128992774059070170, -0.8584487936018656562 ) ) ;
#777 = CARTESIAN_POINT ( 'NONE',  ( 40.00000000000006395, -2.499999999999997335, -20.00000000000000000 ) ) ;
#778 = DIRECTION ( 'NONE',  ( -1.000000000000000000, 1.010728034814421376E-30, 1.090846720500930387E-30 ) ) ;
#779 = CARTESIAN_POINT ( 'NONE',  ( 20.00000000000000000, 10.63631887905125950, -9.927230231572497843 ) ) ;
#780 = DIRECTION ( 'NONE',  ( -1.000000000000000000, 1.010728034814421376E-30, 1.090846720500930387E-30 ) ) ;
#781 = DIRECTION ( 'NONE',  ( 0.000000000000000000, 0.000000000000000000, 1.000000000000000000 ) ) ;
#782 = CARTESIAN_POINT ( 'NONE',  ( -35.00000000000006395, 19.99999999999999645, 2.000000000000006661 ) ) ;
#783 = AXIS2_PLACEMENT_3D ( 'NONE', #10673, #11597, #12572 ) ;
#784 = LINE ( 'NONE', #11558, #3995 ) ;
#785 = DIRECTION ( 'NONE',  ( 0.000000000000000000, 1.000000000000000000, 0.000000000000000000 ) ) ;
#786 = UNCERTAINTY_MEASURE_WITH_UNIT (LENGTH_MEASURE( 1.000000000000000082E-05 ), #10711, 'distance_accuracy_value', 'NONE');
#787 = CARTESIAN_POINT ( 'NONE',  ( 0.000000000000000000, 1.773042676681341856, -3.469446951953614189E-15 ) ) ;
#788 = ORIENTED_EDGE ( 'NONE', *, *, #3741, .F. ) ;
#789 = VECTOR ( 'NONE', #11946, 1000.000000000000114 ) ;
#790 = ORIENTED_EDGE ( 'NONE', *, *, #5569, .F. ) ;
#791 = ORIENTED_EDGE ( 'NONE', *, *, #10760, .F. ) ;
#792 = DIRECTION ( 'NONE',  ( 1.140150527077241873E-30, 0.000000000000000000, -1.000000000000000000 ) ) ;
#793 = DIRECTION ( 'NONE',  ( 0.000000000000000000, 1.177425296209237785E-30, 1.000000000000000000 ) ) ;
#794 = CARTESIAN_POINT ( 'NONE',  ( 33.00000000000001421, 40.41548023366553366, -10.14535464186970870 ) ) ;
#795 = FACE_BOUND ( 'NONE', #2630, .T. ) ;
#796 = ORIENTED_EDGE ( 'NONE', *, *, #6469, .F. ) ;
#797 = FACE_OUTER_BOUND ( 'NONE', #626, .T. ) ;
#798 = CIRCLE ( 'NONE', #8573, 2.800000000000003375 ) ;
#799 = VECTOR ( 'NONE', #9430, 1000.000000000000000 ) ;
#800 = AXIS2_PLACEMENT_3D ( 'NONE', #1062, #6025, #7952 ) ;
#801 = FACE_OUTER_BOUND ( 'NONE', #953, .T. ) ;
#802 = VERTEX_POINT ( 'NONE', #8984 ) ;
#803 = VERTEX_POINT ( 'NONE', #3678 ) ;
#804 = EDGE_CURVE ( 'NONE', #4951, #2162, #7730, .T. ) ;
#805 = CARTESIAN_POINT ( 'NONE',  ( 40.00000000000000711, 11.45997319858344987, -23.64547756539572276 ) ) ;
#806 = ORIENTED_EDGE ( 'NONE', *, *, #12168, .T. ) ;
#807 = ORIENTED_EDGE ( 'NONE', *, *, #3273, .F. ) ;
#808 = AXIS2_PLACEMENT_3D ( 'NONE', #2794, #5790, #11854 ) ;
#809 = FACE_OUTER_BOUND ( 'NONE', #856, .T. ) ;
#810 = COLOUR_RGB ( '', 0.72549020, 0.75294118, 0.79215686) ;
#811 = ORIENTED_EDGE ( 'NONE', *, *, #11377, .F. ) ;
#812 = AXIS2_PLACEMENT_3D ( 'NONE', #8077, #11046, #4086 ) ;
#813 = DIRECTION ( 'NONE',  ( -1.000000000000000000, -5.916456789157575403E-31, 1.577021341797099039E-16 ) ) ;
#814 = CARTESIAN_POINT ( 'NONE',  ( 19.99999999999997868, 6.359055127044386246, 1.682410996215993881 ) ) ;
#815 = VERTEX_POINT ( 'NONE', #5661 ) ;
#816 = AXIS2_PLACEMENT_3D ( 'NONE', #12029, #3339, #7260 ) ;
#817 = DIRECTION ( 'NONE',  ( 0.000000000000000000, 0.000000000000000000, -1.000000000000000000 ) ) ;
#818 =( BOUNDED_SURFACE ( )  B_SPLINE_SURFACE ( 3, 2, ( 
 ( #10960, #7111, #10048 ),
 ( #7993, #2286, #5236 ),
 ( #7303, #11097, #8193 ),
 ( #6136, #3327, #6262 ),
 ( #10173, #274, #11031 ),
 ( #9214, #4333, #12139 ) ),
 .UNSPECIFIED., .F., .F., .F. ) 
 B_SPLINE_SURFACE_WITH_KNOTS ( ( 4, 2, 4 ),
 ( 3, 3 ),
 ( 0.02027752710269158445, 0.02273781595091097299, 0.02519810479913036153 ),
 ( 0.000000000000000000, 1.000000000000000000 ),
 .UNSPECIFIED. ) 
 GEOMETRIC_REPRESENTATION_ITEM ( )  RATIONAL_B_SPLINE_SURFACE ( (
 ( 1.000000000000000000, 0.8047781431712808242, 1.000000000000000000),
 ( 1.000000000000000000, 0.8123773247083928561, 1.000000000000000000),
 ( 1.000000000000000000, 0.8190670192154906326, 1.000000000000000000),
 ( 1.000000000000000000, 0.8192353552912178261, 1.000000000000000000),
 ( 1.000000000000000000, 0.8126132098226828138, 1.000000000000000000),
 ( 1.000000000000000000, 0.8047712465856391439, 1.000000000000000000) ) ) 
 REPRESENTATION_ITEM ( '' )  SURFACE ( )  );
#819 = DIRECTION ( 'NONE',  ( 1.031065855027150586E-29, -1.000000000000000000, 5.551115123125776539E-17 ) ) ;
#820 = AXIS2_PLACEMENT_3D ( 'NONE', #3748, #648, #8441 ) ;
#821 = AXIS2_PLACEMENT_3D ( 'NONE', #5989, #11671, #5736 ) ;
#822 = ORIENTED_EDGE ( 'NONE', *, *, #9458, .T. ) ;
#823 = ORIENTED_EDGE ( 'NONE', *, *, #7750, .T. ) ;
#824 = EDGE_CURVE ( 'NONE', #7005, #11281, #3866, .T. ) ;
#825 = VERTEX_POINT ( 'NONE', #167 ) ;
#826 = APPLICATION_CONTEXT ( 'automotive_design' ) ;
#827 = DIRECTION ( 'NONE',  ( 0.000000000000000000, -0.7818314824680222541, -0.6234898018587429203 ) ) ;
#828 = DIRECTION ( 'NONE',  ( -1.000000000000000000, 0.000000000000000000, -6.982962677686266711E-15 ) ) ;
#829 = ORIENTED_EDGE ( 'NONE', *, *, #12238, .T. ) ;
#830 = DIRECTION ( 'NONE',  ( 0.8660254037844374864, -0.5000000000000018874, 7.395570986446984800E-31 ) ) ;
#831 = AXIS2_PLACEMENT_3D ( 'NONE', #8362, #6370, #6441 ) ;
#832 = FACE_OUTER_BOUND ( 'NONE', #3271, .T. ) ;
#833 = CARTESIAN_POINT ( 'NONE',  ( 1.360585162435131057, -4.061296242128142886, -3.505054077164857951 ) ) ;
#834 = CYLINDRICAL_SURFACE ( 'NONE', #10265, 2.149999999999999023 ) ;
#835 = ORIENTED_EDGE ( 'NONE', *, *, #1795, .F. ) ;
#836 = DIRECTION ( 'NONE',  ( 0.000000000000000000, 0.000000000000000000, -1.000000000000000000 ) ) ;
#837 = VERTEX_POINT ( 'NONE', #4643 ) ;
#838 = EDGE_CURVE ( 'NONE', #4187, #10144, #4093, .T. ) ;
#839 = CARTESIAN_POINT ( 'NONE',  ( 0.000000000000000000, 5.914787828628604416, -4.446941076999666009 ) ) ;
#840 = EDGE_CURVE ( 'NONE', #1206, #1961, #10652, .T. ) ;
#841 = CARTESIAN_POINT ( 'NONE',  ( 2.100000000000035172, -3.469446951953614189E-15, -4.694516984716123886 ) ) ;
#842 = DIRECTION ( 'NONE',  ( -1.000000000000000000, 1.010728034814421376E-30, 1.090846720500930387E-30 ) ) ;
#843 = EDGE_CURVE ( 'NONE', #245, #9681, #6582, .T. ) ;
#844 = CARTESIAN_POINT ( 'NONE',  ( 19.99999999999997868, 4.192831774279055068, -4.965597920955358902 ) ) ;
#845 = AXIS2_PLACEMENT_3D ( 'NONE', #4474, #8392, #8331 ) ;
#846 = CARTESIAN_POINT ( 'NONE',  ( 19.99999999999999645, 0.000000000000000000, 0.000000000000000000 ) ) ;
#847 = DIRECTION ( 'NONE',  ( 0.000000000000000000, 1.000000000000000000, 0.000000000000000000 ) ) ;
#848 = FACE_OUTER_BOUND ( 'NONE', #7283, .T. ) ;
#849 = CARTESIAN_POINT ( 'NONE',  ( 0.000000000000000000, -0.8135880386782442519, -6.527339685683426929 ) ) ;
#850 = DIRECTION ( 'NONE',  ( 1.000000000000000000, -0.000000000000000000, -6.938893903907228378E-17 ) ) ;
#851 = CIRCLE ( 'NONE', #2312, 3.300000000000003375 ) ;
#852 = EDGE_CURVE ( 'NONE', #1792, #10769, #12505, .T. ) ;
#853 = CARTESIAN_POINT ( 'NONE',  ( 6.000000000000000000, 49.63999999999998636, -5.000000000000000888 ) ) ;
#854 = EDGE_CURVE ( 'NONE', #1393, #11974, #1403, .T. ) ;
#855 = AXIS2_PLACEMENT_3D ( 'NONE', #331, #8316, #6321 ) ;
#856 = EDGE_LOOP ( 'NONE', ( #6670, #8268, #11592, #5004 ) ) ;
#857 = ORIENTED_EDGE ( 'NONE', *, *, #6520, .F. ) ;
#858 = CARTESIAN_POINT ( 'NONE',  ( 19.99999999999999645, -0.4733669331952357062, 6.481737787550290619 ) ) ;
#859 = DIRECTION ( 'NONE',  ( 1.000000000000000000, -1.010728034814421376E-30, -1.090846720500930387E-30 ) ) ;
#860 = LINE ( 'NONE', #9730, #6762 ) ;
#861 = DIRECTION ( 'NONE',  ( 1.000000000000000000, 1.849040895279789448E-31, -6.938893903907224680E-17 ) ) ;
#862 = ORIENTED_EDGE ( 'NONE', *, *, #6687, .F. ) ;
#863 = DIRECTION ( 'NONE',  ( -1.000000000000000000, -5.916456789157575403E-31, 1.577021341797098793E-16 ) ) ;
#864 = CARTESIAN_POINT ( 'NONE',  ( 19.99999999999999645, -4.707829255731172502, -5.709320773864600795 ) ) ;
#865 = VERTEX_POINT ( 'NONE', #8021 ) ;
#866 = ORIENTED_EDGE ( 'NONE', *, *, #11872, .F. ) ;
#867 = CYLINDRICAL_SURFACE ( 'NONE', #7181, 2.800000000000003819 ) ;
#868 = ORIENTED_EDGE ( 'NONE', *, *, #10999, .F. ) ;
#869 = ORIENTED_EDGE ( 'NONE', *, *, #6126, .F. ) ;
#870 = SURFACE_STYLE_USAGE ( .BOTH. , #3124 ) ;
#871 = CIRCLE ( 'NONE', #8061, 7.400000000000011902 ) ;
#872 = EDGE_CURVE ( 'NONE', #5322, #574, #6832, .T. ) ;
#873 = AXIS2_PLACEMENT_3D ( 'NONE', #3980, #951, #2044 ) ;
#874 = LINE ( 'NONE', #3908, #9431 ) ;
#875 = EDGE_LOOP ( 'NONE', ( #207, #9419, #4311, #1916, #9816, #12149, #7760, #7885, #10727, #12727 ) ) ;
#876 = LINE ( 'NONE', #4088, #7398 ) ;
#877 = EDGE_CURVE ( 'NONE', #2957, #11940, #8218, .T. ) ;
#878 = LINE ( 'NONE', #9620, #1011 ) ;
#879 = EDGE_LOOP ( 'NONE', ( #430, #5834, #11812, #1139 ) ) ;
#880 = CARTESIAN_POINT ( 'NONE',  ( 3.469446951953614189E-14, -3.469446951953614189E-15, -5.000000000000011546 ) ) ;
#881 = DIRECTION ( 'NONE',  ( 1.000000000000000000, 1.848892746611742259E-31, -1.154721252774410375E-34 ) ) ;
#882 = AXIS2_PLACEMENT_3D ( 'NONE', #6214, #8019, #11052 ) ;
#883 = VECTOR ( 'NONE', #7862, 1000.000000000000000 ) ;
#884 = AXIS2_PLACEMENT_3D ( 'NONE', #10014, #5142, #9121 ) ;
#885 = ORIENTED_EDGE ( 'NONE', *, *, #5888, .F. ) ;
#886 = ORIENTED_EDGE ( 'NONE', *, *, #164, .F. ) ;
#887 = ORIENTED_EDGE ( 'NONE', *, *, #8327, .T. ) ;
#888 = CARTESIAN_POINT ( 'NONE',  ( 0.000000000000000000, -0.8865213383406691516, 1.535500000000002085 ) ) ;
#889 = ORIENTED_EDGE ( 'NONE', *, *, #10751, .F. ) ;
#890 = FACE_OUTER_BOUND ( 'NONE', #6082, .T. ) ;
#891 = SHAPE_REPRESENTATION ( 'upper roller_ISO - Spur gear 0.4M 35T 20PA 20FW ---S35A75H50L5.0N', ( #12422 ), #639 ) ;
#892 = ORIENTED_EDGE ( 'NONE', *, *, #6007, .F. ) ;
#893 = FACE_BOUND ( 'NONE', #708, .T. ) ;
#894 = EDGE_CURVE ( 'NONE', #2378, #9789, #4768, .T. ) ;
#895 = EDGE_CURVE ( 'NONE', #6619, #5731, #4929, .T. ) ;
#896 = EDGE_CURVE ( 'NONE', #8586, #9298, #4700, .T. ) ;
#897 = CARTESIAN_POINT ( 'NONE',  ( 19.99999999999999645, 0.000000000000000000, 0.000000000000000000 ) ) ;
#898 = AXIS2_PLACEMENT_3D ( 'NONE', #10933, #5615, #7679 ) ;
#899 = DIRECTION ( 'NONE',  ( 1.000000000000000000, 0.000000000000000000, 0.000000000000000000 ) ) ;
#900 = ORIENTED_EDGE ( 'NONE', *, *, #1095, .F. ) ;
#901 = CYLINDRICAL_SURFACE ( 'NONE', #2276, 2.800000000000003819 ) ;
#902 = EDGE_LOOP ( 'NONE', ( #5113, #5119, #7738, #9992 ) ) ;
#903 = DIRECTION ( 'NONE',  ( 0.000000000000000000, -1.530455820933490821E-32, 1.000000000000000000 ) ) ;
#904 = CIRCLE ( 'NONE', #1315, 2.800000000000002931 ) ;
#905 = DIRECTION ( 'NONE',  ( -1.000000000000000000, 1.010728034814421376E-30, 1.090846720500930387E-30 ) ) ;
#906 = AXIS2_PLACEMENT_3D ( 'NONE', #814, #3973, #10600 ) ;
#907 = CARTESIAN_POINT ( 'NONE',  ( 11.00000000000003375, 12.50000000000000000, -7.673627122167892852E-31 ) ) ;
#908 = DIRECTION ( 'NONE',  ( -1.000000000000000000, 1.010728034814421376E-30, 1.090846720500930387E-30 ) ) ;
#909 = ADVANCED_FACE ( 'NONE', ( #832 ), #12633, .T. ) ;
#910 = CARTESIAN_POINT ( 'NONE',  ( 2.000000000000001776, 1.773042676681338303, 0.000000000000000000 ) ) ;
#911 = DIRECTION ( 'NONE',  ( 1.000000000000000000, 1.849040895279789448E-31, -6.938893903907224680E-17 ) ) ;
#912 = CIRCLE ( 'NONE', #1325, 2.149999999999994138 ) ;
#913 = VECTOR ( 'NONE', #8680, 1000.000000000000000 ) ;
#914 = DIRECTION ( 'NONE',  ( 0.000000000000000000, 0.000000000000000000, 1.000000000000000000 ) ) ;
#915 = DIRECTION ( 'NONE',  ( -1.000000000000000000, -1.081682119347366197E-16, 6.938893903907228378E-17 ) ) ;
#916 = EDGE_CURVE ( 'NONE', #1397, #12171, #5951, .T. ) ;
#917 = CARTESIAN_POINT ( 'NONE',  ( 4.000000000000003553, 2.694222958124189825E-16, 2.199999999999992184 ) ) ;
#918 = AXIS2_PLACEMENT_3D ( 'NONE', #8549, #2515, #3424 ) ;
#919 = ORIENTED_EDGE ( 'NONE', *, *, #10805, .F. ) ;
#920 = VECTOR ( 'NONE', #986, 1000.000000000000000 ) ;
#921 = ORIENTED_EDGE ( 'NONE', *, *, #4079, .T. ) ;
#922 = LINE ( 'NONE', #4918, #1295 ) ;
#923 = CARTESIAN_POINT ( 'NONE',  ( 20.00000000000000000, 8.163911011730665024, -17.95311239921186441 ) ) ;
#924 = DIRECTION ( 'NONE',  ( -0.000000000000000000, -1.000000000000000000, -0.000000000000000000 ) ) ;
#925 = EDGE_CURVE ( 'NONE', #10658, #2655, #357, .T. ) ;
#926 = DIRECTION ( 'NONE',  ( -1.000000000000000000, -5.916456789157575403E-31, 1.577021341797098793E-16 ) ) ;
#927 = VERTEX_POINT ( 'NONE', #7131 ) ;
#928 = LINE ( 'NONE', #7998, #7727 ) ;
#929 = EDGE_CURVE ( 'NONE', #2828, #7514, #2471, .T. ) ;
#930 = CIRCLE ( 'NONE', #7918, 10.00000000000002309 ) ;
#931 = DIRECTION ( 'NONE',  ( 0.000000000000000000, 0.000000000000000000, -1.000000000000000000 ) ) ;
#932 = CARTESIAN_POINT ( 'NONE',  ( 19.99999999999999645, -6.577476285968329783, 0.06996125000489905599 ) ) ;
#933 = EDGE_LOOP ( 'NONE', ( #2197, #5461, #5972, #6284 ) ) ;
#934 = VECTOR ( 'NONE', #593, 1000.000000000000000 ) ;
#935 = EDGE_LOOP ( 'NONE', ( #8597, #11513, #1513, #7375, #1039 ) ) ;
#936 = DIRECTION ( 'NONE',  ( 0.000000000000000000, 0.000000000000000000, 1.000000000000000000 ) ) ;
#937 = VERTEX_POINT ( 'NONE', #12282 ) ;
#938 = VERTEX_POINT ( 'NONE', #7194 ) ;
#939 = FACE_OUTER_BOUND ( 'NONE', #66, .T. ) ;
#940 = ORIENTED_EDGE ( 'NONE', *, *, #11784, .F. ) ;
#941 = DIRECTION ( 'NONE',  ( -1.000000000000000000, 0.000000000000000000, 0.000000000000000000 ) ) ;
#942 = LINE ( 'NONE', #12743, #3570 ) ;
#943 = ORIENTED_EDGE ( 'NONE', *, *, #1608, .T. ) ;
#944 = VECTOR ( 'NONE', #3056, 1000.000000000000000 ) ;
#945 = CARTESIAN_POINT ( 'NONE',  ( 5.560781378645605955, -3.469446951953614189E-15, -4.000000000000010658 ) ) ;
#946 = DIRECTION ( 'NONE',  ( -1.081682119347366197E-16, 1.000000000000000000, 0.000000000000000000 ) ) ;
#947 = ORIENTED_EDGE ( 'NONE', *, *, #1314, .T. ) ;
#948 = ADVANCED_FACE ( 'NONE', ( #3466 ), #484, .T. ) ;
#949 = ORIENTED_EDGE ( 'NONE', *, *, #6883, .T. ) ;
#950 = ORIENTED_EDGE ( 'NONE', *, *, #1873, .F. ) ;
#951 = DIRECTION ( 'NONE',  ( -1.848892746611746419E-31, -1.000000000000000000, 3.250006781153460502E-32 ) ) ;
#952 = AXIS2_PLACEMENT_3D ( 'NONE', #4622, #4428, #10272 ) ;
#953 = EDGE_LOOP ( 'NONE', ( #2112, #9197, #11094, #219, #1705 ) ) ;
#954 = LINE ( 'NONE', #3738, #5356 ) ;
#955 = VERTEX_POINT ( 'NONE', #8214 ) ;
#956 = CIRCLE ( 'NONE', #8157, 2.800000000000003819 ) ;
#957 = CIRCLE ( 'NONE', #334, 2.800000000000003819 ) ;
#958 = DIRECTION ( 'NONE',  ( 0.000000000000000000, 1.000000000000000000, 0.000000000000000000 ) ) ;
#959 = PLANE ( 'NONE',  #7403 ) ;
#960 = ORIENTED_EDGE ( 'NONE', *, *, #1412, .F. ) ;
#961 = DIRECTION ( 'NONE',  ( 0.000000000000000000, 0.000000000000000000, 1.000000000000000000 ) ) ;
#962 = VERTEX_POINT ( 'NONE', #5251 ) ;
#963 = FACE_OUTER_BOUND ( 'NONE', #622, .T. ) ;
#964 = EDGE_CURVE ( 'NONE', #11709, #1279, #2236, .T. ) ;
#965 = AXIS2_PLACEMENT_3D ( 'NONE', #6571, #4696, #8492 ) ;
#966 = ADVANCED_FACE ( 'NONE', ( #11308 ), #6217, .T. ) ;
#967 = VECTOR ( 'NONE', #3055, 1000.000000000000000 ) ;
#968 = AXIS2_PLACEMENT_3D ( 'NONE', #6719, #5802, #8710 ) ;
#969 = DIRECTION ( 'NONE',  ( -1.000000000000000000, 1.010728034814421376E-30, 1.090846720500930387E-30 ) ) ;
#970 = DIRECTION ( 'NONE',  ( 7.169062767534772867E-17, -0.02142605311579142552, 0.9997704357740727632 ) ) ;
#971 = LINE ( 'NONE', #75, #10203 ) ;
#972 = DIRECTION ( 'NONE',  ( -1.000000000000000000, 1.010728034814421376E-30, 1.090846720500930387E-30 ) ) ;
#973 = CARTESIAN_POINT ( 'NONE',  ( 0.000000000000000000, 0.000000000000000000, 0.000000000000000000 ) ) ;
#974 = LINE ( 'NONE', #5040, #7987 ) ;
#975 = CIRCLE ( 'NONE', #6121, 2.000000000000000888 ) ;
#976 = CARTESIAN_POINT ( 'NONE',  ( 19.99999999999997868, 6.557268578288205418, -0.5199208220221240850 ) ) ;
#977 = DIRECTION ( 'NONE',  ( 1.140150527077241873E-30, 0.000000000000000000, -1.000000000000000000 ) ) ;
#978 = EDGE_CURVE ( 'NONE', #3412, #10716, #5341, .T. ) ;
#979 = ORIENTED_EDGE ( 'NONE', *, *, #6966, .F. ) ;
#980 = ORIENTED_EDGE ( 'NONE', *, *, #10516, .T. ) ;
#981 = FACE_OUTER_BOUND ( 'NONE', #3039, .T. ) ;
#982 = CARTESIAN_POINT ( 'NONE',  ( 2.000000000000091926, 0.8865213383406691516, -1.535500000000002085 ) ) ;
#983 = DIRECTION ( 'NONE',  ( -1.000000000000000000, 1.010728034814421376E-30, 1.090846720500930387E-30 ) ) ;
#984 = DIRECTION ( 'NONE',  ( 0.000000000000000000, 0.4338837391175524583, 0.9009688679024216995 ) ) ;
#985 = ORIENTED_EDGE ( 'NONE', *, *, #1695, .T. ) ;
#986 = DIRECTION ( 'NONE',  ( -1.000000000000000000, 1.010728034814421376E-30, 1.090846720500930387E-30 ) ) ;
#987 = FACE_OUTER_BOUND ( 'NONE', #6274, .T. ) ;
#988 = DIRECTION ( 'NONE',  ( -1.000000000000000000, 1.010728034814421376E-30, 1.090846720500930387E-30 ) ) ;
#989 = ORIENTED_EDGE ( 'NONE', *, *, #9398, .F. ) ;
#990 = ORIENTED_EDGE ( 'NONE', *, *, #11430, .F. ) ;
#991 = CARTESIAN_POINT ( 'NONE',  ( -30.00000000000000000, -19.99999999999999645, 0.000000000000000000 ) ) ;
#992 = VERTEX_POINT ( 'NONE', #3280 ) ;
#993 = AXIS2_PLACEMENT_3D ( 'NONE', #148, #7994, #12663 ) ;
#994 = ORIENTED_EDGE ( 'NONE', *, *, #11737, .T. ) ;
#995 = PRODUCT_CONTEXT ( 'NONE', #12106, 'mechanical' ) ;
#996 = ADVANCED_FACE ( 'NONE', ( #11245 ), #1320, .T. ) ;
#997 = EDGE_CURVE ( 'NONE', #3286, #9151, #3483, .T. ) ;
#998 = DIRECTION ( 'NONE',  ( 0.000000000000000000, 0.000000000000000000, 1.000000000000000000 ) ) ;
#999 = ORIENTED_EDGE ( 'NONE', *, *, #8325, .F. ) ;
#1000 = ADVANCED_FACE ( 'NONE', ( #9168 ), #11180, .F. ) ;
#1001 = CARTESIAN_POINT ( 'NONE',  ( 0.1999999999999987899, 4.286263797015736595E-16, -3.500000000000017319 ) ) ;
#1002 = DIRECTION ( 'NONE',  ( -1.000000000000000000, 1.010728034814421376E-30, 1.090846720500930387E-30 ) ) ;
#1003 = ORIENTED_EDGE ( 'NONE', *, *, #4683, .T. ) ;
#1004 = VECTOR ( 'NONE', #9771, 1000.000000000000000 ) ;
#1005 = CARTESIAN_POINT ( 'NONE',  ( 3.469446951953614189E-14, -3.469446951953614189E-15, -5.000000000000011546 ) ) ;
#1006 = EDGE_CURVE ( 'NONE', #7962, #2242, #4285, .T. ) ;
#1007 = DIRECTION ( 'NONE',  ( -1.000000000000000000, 1.010728034814421376E-30, 1.090846720500930387E-30 ) ) ;
#1008 = EDGE_LOOP ( 'NONE', ( #5764, #10223, #12292, #11299 ) ) ;
#1009 = ORIENTED_EDGE ( 'NONE', *, *, #2005, .F. ) ;
#1010 = CIRCLE ( 'NONE', #1830, 7.400000000000011902 ) ;
#1011 = VECTOR ( 'NONE', #11836, 1000.000000000000000 ) ;
#1012 = ORIENTED_EDGE ( 'NONE', *, *, #3749, .F. ) ;
#1013 =( GEOMETRIC_REPRESENTATION_CONTEXT ( 3 ) GLOBAL_UNCERTAINTY_ASSIGNED_CONTEXT ( ( #8516 ) ) GLOBAL_UNIT_ASSIGNED_CONTEXT ( ( #5432, #1437, #12211 ) ) REPRESENTATION_CONTEXT ( 'NONE', 'WORKASPACE' ) );
#1014 = CARTESIAN_POINT ( 'NONE',  ( 0.000000000000000000, 0.000000000000000000, 0.000000000000000000 ) ) ;
#1015 = AXIS2_PLACEMENT_3D ( 'NONE', #1478, #5410, #7534 ) ;
#1016 = ORIENTED_EDGE ( 'NONE', *, *, #5333, .F. ) ;
#1017 = DIRECTION ( 'NONE',  ( -1.000000000000000000, 1.010728034814421376E-30, 1.090846720500930387E-30 ) ) ;
#1018 = ORIENTED_EDGE ( 'NONE', *, *, #12161, .F. ) ;
#1019 = CIRCLE ( 'NONE', #808, 2.149999999999994138 ) ;
#1020 = CIRCLE ( 'NONE', #12562, 2.800000000000003819 ) ;
#1021 = CIRCLE ( 'NONE', #8427, 4.000000000000000000 ) ;
#1022 = CARTESIAN_POINT ( 'NONE',  ( 0.6640947660595887259, -4.471078309994368283, -3.602146406945785806 ) ) ;
#1023 = CARTESIAN_POINT ( 'NONE',  ( 33.00000000000000711, 39.92642927056392210, -24.05727230799563898 ) ) ;
#1024 = ORIENTED_EDGE ( 'NONE', *, *, #8317, .T. ) ;
#1025 = CYLINDRICAL_SURFACE ( 'NONE', #12746, 2.800000000000003819 ) ;
#1026 = ORIENTED_EDGE ( 'NONE', *, *, #306, .F. ) ;
#1027 = FACE_OUTER_BOUND ( 'NONE', #9727, .T. ) ;
#1028 = AXIS2_PLACEMENT_3D ( 'NONE', #11252, #426, #7264 ) ;
#1029 = AXIS2_PLACEMENT_3D ( 'NONE', #9712, #905, #5865 ) ;
#1030 = DIRECTION ( 'NONE',  ( 0.000000000000000000, 0.000000000000000000, 1.000000000000000000 ) ) ;
#1031 = CARTESIAN_POINT ( 'NONE',  ( 40.00000000000000711, 14.50364731389636574, -24.59751492040896892 ) ) ;
#1032 = CYLINDRICAL_SURFACE ( 'NONE', #7953, 6.499000000000010324 ) ;
#1033 = DIRECTION ( 'NONE',  ( -1.000000000000000000, -1.031065855027150586E-29, 2.218671295934095703E-30 ) ) ;
#1034 = CARTESIAN_POINT ( 'NONE',  ( -7.888106377466153063, -30.00000000000000000, -1.333333333333333703 ) ) ;
#1035 = COLOUR_RGB ( '', 0.40784314, 0.44705882, 0.49803922) ;
#1036 = LINE ( 'NONE', #4975, #8822 ) ;
#1037 = CYLINDRICAL_SURFACE ( 'NONE', #1434, 10.00000000000000000 ) ;
#1038 = DIRECTION ( 'NONE',  ( 0.000000000000000000, 0.000000000000000000, -1.000000000000000000 ) ) ;
#1039 = ORIENTED_EDGE ( 'NONE', *, *, #3460, .T. ) ;
#1040 = EDGE_LOOP ( 'NONE', ( #4220, #9747, #9061, #3791, #6995 ) ) ;
#1041 = CARTESIAN_POINT ( 'NONE',  ( 19.99999999999999645, -1.623118704078951202, 6.293050665016855838 ) ) ;
#1042 = PLANE ( 'NONE',  #9781 ) ;
#1043 = DIRECTION ( 'NONE',  ( 1.000000000000000000, -6.162975822039154730E-33, -4.563833282352349791E-17 ) ) ;
#1044 = DIRECTION ( 'NONE',  ( -1.000000000000000000, 1.010728034814421376E-30, 1.090846720500930387E-30 ) ) ;
#1045 = VERTEX_POINT ( 'NONE', #5196 ) ;
#1046 = EDGE_CURVE ( 'NONE', #3737, #8175, #12317, .T. ) ;
#1047 = DIRECTION ( 'NONE',  ( 1.000000000000000000, -1.010728034814421376E-30, -1.090846720500930387E-30 ) ) ;
#1048 = ADVANCED_FACE ( 'NONE', ( #9113 ), #5377, .T. ) ;
#1049 = ADVANCED_FACE ( 'NONE', ( #8082 ), #8340, .T. ) ;
#1050 = DIRECTION ( 'NONE',  ( -1.140150527077241873E-30, 0.000000000000000000, 1.000000000000000000 ) ) ;
#1051 = CIRCLE ( 'NONE', #7650, 2.800000000000002931 ) ;
#1052 = DIRECTION ( 'NONE',  ( -7.818312609239974136E-30, -0.8660254037844390407, -0.4999999999999992784 ) ) ;
#1053 = VERTEX_POINT ( 'NONE', #3220 ) ;
#1054 = EDGE_LOOP ( 'NONE', ( #10463, #2615, #10847, #11911 ) ) ;
#1055 = CARTESIAN_POINT ( 'NONE',  ( 5.603754474795991474E-15, 4.647089433458983621, -3.572167766733752359 ) ) ;
#1056 = ORIENTED_EDGE ( 'NONE', *, *, #12288, .F. ) ;
#1057 = VERTEX_POINT ( 'NONE', #4225 ) ;
#1058 = APPLICATION_PROTOCOL_DEFINITION ( 'draft international standard', 'automotive_design', 1998, #826 ) ;
#1059 = ADVANCED_FACE ( 'NONE', ( #5313 ), #9230, .T. ) ;
#1060 = DIRECTION ( 'NONE',  ( 1.000000000000000000, 5.916456789157575403E-31, -1.224646799147352714E-16 ) ) ;
#1061 = ORIENTED_EDGE ( 'NONE', *, *, #2666, .T. ) ;
#1062 = CARTESIAN_POINT ( 'NONE',  ( 28.61000000000001009, 3.469446951953614189E-15, 0.000000000000000000 ) ) ;
#1063 = DIRECTION ( 'NONE',  ( 0.000000000000000000, -0.9989930665413151445, 0.04486483035050446017 ) ) ;
#1064 = AXIS2_PLACEMENT_3D ( 'NONE', #8443, #3323, #10225 ) ;
#1065 = ORIENTED_EDGE ( 'NONE', *, *, #4126, .F. ) ;
#1066 = CARTESIAN_POINT ( 'NONE',  ( 19.99999999999999645, 0.000000000000000000, 0.000000000000000000 ) ) ;
#1067 = APPLICATION_CONTEXT ( 'automotive_design' ) ;
#1068 = CARTESIAN_POINT ( 'NONE',  ( 19.99999999999999645, -6.213893036447794671, -1.903820982021606989 ) ) ;
#1069 = CLOSED_SHELL ( 'NONE', ( #11145, #12631, #7196, #1644, #5684, #7981, #1755, #9394, #2322, #7154, #9459, #2680, #12532, #10758, #5653, #8693, #9274, #1388, #4949, #6562, #506, #1391, #8396, #5578, #8161, #6105, #5540, #7022, #10570, #4903, #4196, #11952 ) ) ;
#1070 = ORIENTED_EDGE ( 'NONE', *, *, #3986, .T. ) ;
#1071 = ORIENTED_EDGE ( 'NONE', *, *, #6349, .F. ) ;
#1072 = CIRCLE ( 'NONE', #4778, 3.500000000000000000 ) ;
#1073 = ORIENTED_EDGE ( 'NONE', *, *, #12643, .F. ) ;
#1074 = CARTESIAN_POINT ( 'NONE',  ( 19.99999999999997868, 6.424561140605097087, -0.9808237102696195642 ) ) ;
#1075 = EDGE_CURVE ( 'NONE', #9359, #4176, #10389, .T. ) ;
#1076 = DIRECTION ( 'NONE',  ( 1.380506584136768733E-30, -0.5128992774058948045, -0.8584487936018728726 ) ) ;
#1077 = VERTEX_POINT ( 'NONE', #673 ) ;
#1078 = PLANE ( 'NONE',  #5936 ) ;
#1079 = ORIENTED_EDGE ( 'NONE', *, *, #5419, .F. ) ;
#1080 = DIRECTION ( 'NONE',  ( 0.000000000000000000, 0.08963930890342672320, 0.9959742939952396235 ) ) ;
#1081 = CIRCLE ( 'NONE', #2755, 1.535500000000001863 ) ;
#1082 = CIRCLE ( 'NONE', #2757, 19.99999999999998934 ) ;
#1083 = ADVANCED_FACE ( 'NONE', ( #549 ), #5630, .T. ) ;
#1084 = ADVANCED_FACE ( 'NONE', ( #3710 ), #10322, .T. ) ;
#1085 = CYLINDRICAL_SURFACE ( 'NONE', #3410, 2.800000000000003819 ) ;
#1086 = DIRECTION ( 'NONE',  ( 0.000000000000000000, -1.530455820933490821E-32, 1.000000000000000000 ) ) ;
#1087 = ORIENTED_EDGE ( 'NONE', *, *, #2568, .T. ) ;
#1088 = DIRECTION ( 'NONE',  ( 1.848892746611746419E-31, 1.000000000000000000, -3.250006781153460502E-32 ) ) ;
#1089 = AXIS2_PLACEMENT_3D ( 'NONE', #12158, #10982, #8210 ) ;
#1090 = VERTEX_POINT ( 'NONE', #1574 ) ;
#1091 = LINE ( 'NONE', #8882, #6645 ) ;
#1092 =( LENGTH_UNIT ( ) NAMED_UNIT ( * ) SI_UNIT ( .MILLI., .METRE. ) );
#1093 = CARTESIAN_POINT ( 'NONE',  ( 15.00000000000003375, -12.49999999999999645, 3.994800001834461867E-31 ) ) ;
#1094 = DIRECTION ( 'NONE',  ( 1.848892746611746419E-31, 1.000000000000000000, -3.250006781153460502E-32 ) ) ;
#1095 = EDGE_CURVE ( 'NONE', #3948, #3079, #5308, .T. ) ;
#1096 = VECTOR ( 'NONE', #6134, 1000.000000000000000 ) ;
#1097 = LINE ( 'NONE', #6364, #1940 ) ;
#1098 = LINE ( 'NONE', #2070, #967 ) ;
#1099 = CARTESIAN_POINT ( 'NONE',  ( 11.00000000000001599, 19.99999999999999645, 12.00000000000003020 ) ) ;
#1100 = CARTESIAN_POINT ( 'NONE',  ( 2.000000000000001776, 0.8865213383406727043, 1.535499999999998755 ) ) ;
#1101 = DIRECTION ( 'NONE',  ( 1.238279320584846685E-16, -0.9554649393887560960, 0.2951046417778627751 ) ) ;
#1102 = CARTESIAN_POINT ( 'NONE',  ( 0.000000000000000000, -7.258495115966566047, -1.440225208600910634 ) ) ;
#1103 = EDGE_CURVE ( 'NONE', #8313, #4963, #12522, .T. ) ;
#1104 = VECTOR ( 'NONE', #11982, 1000.000000000000000 ) ;
#1105 = EDGE_LOOP ( 'NONE', ( #9618, #8342, #10391, #889 ) ) ;
#1106 = CARTESIAN_POINT ( 'NONE',  ( 19.99999999999999645, -6.310777386698697811, -1.552768423021409161 ) ) ;
#1107 = FACE_OUTER_BOUND ( 'NONE', #1947, .T. ) ;
#1108 = DIRECTION ( 'NONE',  ( 1.031682152609352680E-29, 1.000000000000000000, -1.498801083243958569E-15 ) ) ;
#1109 = DIRECTION ( 'NONE',  ( 0.000000000000000000, 0.000000000000000000, -1.000000000000000000 ) ) ;
#1110 = CARTESIAN_POINT ( 'NONE',  ( 19.99999999999999645, 0.000000000000000000, 0.000000000000000000 ) ) ;
#1111 = ORIENTED_EDGE ( 'NONE', *, *, #9158, .T. ) ;
#1112 = AXIS2_PLACEMENT_3D ( 'NONE', #1368, #344, #1244 ) ;
#1113 = CARTESIAN_POINT ( 'NONE',  ( 0.000000000000000000, 0.000000000000000000, 0.000000000000000000 ) ) ;
#1114 = EDGE_CURVE ( 'NONE', #11498, #6729, #11901, .T. ) ;
#1115 = LINE ( 'NONE', #8969, #5641 ) ;
#1116 = PRODUCT_DEFINITION_SHAPE ( 'NONE', 'NONE',  #12761 ) ;
#1117 = ADVANCED_BREP_SHAPE_REPRESENTATION ( '', ( #10152, #12422 ), #639 ) ;
#1118 = CYLINDRICAL_SURFACE ( 'NONE', #4514, 2.149999999999999023 ) ;
#1119 = ORIENTED_EDGE ( 'NONE', *, *, #12538, .F. ) ;
#1120 = ORIENTED_EDGE ( 'NONE', *, *, #3514, .F. ) ;
#1121 = CARTESIAN_POINT ( 'NONE',  ( 19.99999999999999645, 7.358375340957004518, -0.7837807994560894720 ) ) ;
#1122 = ORIENTED_EDGE ( 'NONE', *, *, #9718, .T. ) ;
#1123 = AXIS2_PLACEMENT_3D ( 'NONE', #10087, #11984, #5089 ) ;
#1124 = ORIENTED_EDGE ( 'NONE', *, *, #7748, .T. ) ;
#1125 = PRODUCT_CONTEXT ( 'NONE', #2144, 'mechanical' ) ;
#1126 = CIRCLE ( 'NONE', #4005, 2.149999999999999023 ) ;
#1127 = ADVANCED_FACE ( 'NONE', ( #5693 ), #5574, .F. ) ;
#1128 = CARTESIAN_POINT ( 'NONE',  ( -10.00000000000000178, 0.000000000000000000, 0.000000000000000000 ) ) ;
#1129 = ADVANCED_FACE ( 'NONE', ( #11502 ), #735, .F. ) ;
#1130 = EDGE_LOOP ( 'NONE', ( #12366, #1473, #8778, #5940 ) ) ;
#1131 = CARTESIAN_POINT ( 'NONE',  ( 20.00000000000000355, 19.99999999999999645, -12.00000000000000000 ) ) ;
#1132 = DIRECTION ( 'NONE',  ( -1.000000000000000000, 1.010728034814421376E-30, 1.090846720500930387E-30 ) ) ;
#1133 = ORIENTED_EDGE ( 'NONE', *, *, #3535, .F. ) ;
#1134 = DIRECTION ( 'NONE',  ( -1.000000000000000000, 0.000000000000000000, 0.000000000000000000 ) ) ;
#1135 = DIRECTION ( 'NONE',  ( -1.000000000000000000, 1.010728034814421376E-30, 1.090846720500930387E-30 ) ) ;
#1136 = FACE_OUTER_BOUND ( 'NONE', #9598, .T. ) ;
#1137 = AXIS2_PLACEMENT_3D ( 'NONE', #7402, #571, #10345 ) ;
#1138 = VECTOR ( 'NONE', #1770, 1000.000000000000000 ) ;
#1139 = ORIENTED_EDGE ( 'NONE', *, *, #8439, .F. ) ;
#1140 = ORIENTED_EDGE ( 'NONE', *, *, #9304, .T. ) ;
#1141 = VERTEX_POINT ( 'NONE', #1767 ) ;
#1142 = EDGE_LOOP ( 'NONE', ( #2486, #10917, #3865, #8337 ) ) ;
#1143 = CARTESIAN_POINT ( 'NONE',  ( 9.999999999999994671, -6.289597356626513758, 3.898841506334516094 ) ) ;
#1144 = CARTESIAN_POINT ( 'NONE',  ( -0.5449313310647205810, -4.304185902836956679, -3.316620875264007839 ) ) ;
#1145 = EDGE_CURVE ( 'NONE', #1407, #11320, #6564, .T. ) ;
#1146 = ORIENTED_EDGE ( 'NONE', *, *, #9111, .F. ) ;
#1147 = CIRCLE ( 'NONE', #10169, 5.560781378645573980 ) ;
#1148 = DIRECTION ( 'NONE',  ( -1.000000000000000000, 1.010728034814421376E-30, 1.090846720500930387E-30 ) ) ;
#1149 = ORIENTED_EDGE ( 'NONE', *, *, #7544, .T. ) ;
#1150 = DIRECTION ( 'NONE',  ( 0.000000000000000000, 0.9510565162951545304, -0.3090169943749445092 ) ) ;
#1151 = DIRECTION ( 'NONE',  ( -1.000000000000000000, 1.010728034814421376E-30, 1.090846720500930387E-30 ) ) ;
#1152 = CARTESIAN_POINT ( 'NONE',  ( 40.00000000000000711, 8.524476791110680907, -16.77732469694377926 ) ) ;
#1153 = VERTEX_POINT ( 'NONE', #9602 ) ;
#1154 = FACE_OUTER_BOUND ( 'NONE', #7783, .T. ) ;
#1155 = ORIENTED_EDGE ( 'NONE', *, *, #3496, .F. ) ;
#1156 = DIRECTION ( 'NONE',  ( -4.930380657631325535E-31, -1.000000000000000000, -1.177425296209239362E-30 ) ) ;
#1157 = EDGE_CURVE ( 'NONE', #3414, #5639, #2871, .T. ) ;
#1158 = CARTESIAN_POINT ( 'NONE',  ( 40.00000000000006395, 1.290960574571364216E-15, -20.00000000000000000 ) ) ;
#1159 = EDGE_CURVE ( 'NONE', #8279, #10901, #583, .T. ) ;
#1160 = AXIS2_PLACEMENT_3D ( 'NONE', #8965, #8902, #9025 ) ;
#1161 = DIRECTION ( 'NONE',  ( -1.140150527077241873E-30, 0.000000000000000000, 1.000000000000000000 ) ) ;
#1162 = AXIS2_PLACEMENT_3D ( 'NONE', #2759, #10321, #6545 ) ;
#1163 = CARTESIAN_POINT ( 'NONE',  ( 20.00000000000000000, 15.24625277455639072, -6.248133273622503481 ) ) ;
#1164 = EDGE_CURVE ( 'NONE', #3630, #11388, #11076, .T. ) ;
#1165 = DIRECTION ( 'NONE',  ( 0.000000000000000000, 0.000000000000000000, -1.000000000000000000 ) ) ;
#1166 = DIRECTION ( 'NONE',  ( 0.000000000000000000, 0.000000000000000000, -1.000000000000000000 ) ) ;
#1167 = CARTESIAN_POINT ( 'NONE',  ( 6.000000000000000000, 49.63999999999998636, -13.00000000000000178 ) ) ;
#1168 = CIRCLE ( 'NONE', #4253, 2.800000000000002931 ) ;
#1169 = AXIS2_PLACEMENT_3D ( 'NONE', #8125, #4140, #8057 ) ;
#1170 = DIRECTION ( 'NONE',  ( 0.000000000000000000, 0.000000000000000000, -1.000000000000000000 ) ) ;
#1171 = FILL_AREA_STYLE ('',( #3782 ) ) ;
#1172 = EDGE_LOOP ( 'NONE', ( #10214, #1741, #1308, #6409 ) ) ;
#1173 = CARTESIAN_POINT ( 'NONE',  ( 9.999999999999994671, -7.399010254356641170, -0.1210258481700032807 ) ) ;
#1174 = DIRECTION ( 'NONE',  ( 1.000000000000000000, 1.031065855027150586E-29, 2.218671295934092550E-30 ) ) ;
#1175 = CYLINDRICAL_SURFACE ( 'NONE', #11875, 2.800000000000003819 ) ;
#1176 = DIRECTION ( 'NONE',  ( -4.930380657631325535E-31, -1.000000000000000000, -1.177425296209239362E-30 ) ) ;
#1177 = DIRECTION ( 'NONE',  ( 0.000000000000000000, 0.000000000000000000, 1.000000000000000000 ) ) ;
#1178 = ORIENTED_EDGE ( 'NONE', *, *, #2514, .F. ) ;
#1179 = AXIS2_PLACEMENT_3D ( 'NONE', #8679, #6694, #7716 ) ;
#1180 = CARTESIAN_POINT ( 'NONE',  ( 2.727116801252330522E-30, 5.204170427930467826E-15, 2.499999999999999112 ) ) ;
#1181 = CARTESIAN_POINT ( 'NONE',  ( -18.00000000000001421, -30.00000000000001421, 3.000000000000008438 ) ) ;
#1182 = VERTEX_POINT ( 'NONE', #6546 ) ;
#1183 = CARTESIAN_POINT ( 'NONE',  ( 0.000000000000000000, -6.459281472512942379, -1.243290685169453402 ) ) ;
#1184 = ORIENTED_EDGE ( 'NONE', *, *, #4506, .F. ) ;
#1185 = ORIENTED_EDGE ( 'NONE', *, *, #1164, .F. ) ;
#1186 = SHAPE_DEFINITION_REPRESENTATION ( #517, #3471 ) ;
#1187 = LINE ( 'NONE', #7949, #12349 ) ;
#1188 = VERTEX_POINT ( 'NONE', #7564 ) ;
#1189 = LINE ( 'NONE', #9109, #590 ) ;
#1190 = DIRECTION ( 'NONE',  ( 1.000000000000000000, -0.000000000000000000, -6.938893903907228378E-17 ) ) ;
#1191 = VERTEX_POINT ( 'NONE', #794 ) ;
#1192 = DIRECTION ( 'NONE',  ( 1.000000000000000000, 1.081682119347366197E-16, -6.938893903907228378E-17 ) ) ;
#1193 = FACE_BOUND ( 'NONE', #4343, .T. ) ;
#1194 = CARTESIAN_POINT ( 'NONE',  ( -10.00000000000000178, 0.000000000000000000, 0.000000000000000000 ) ) ;
#1195 = EDGE_CURVE ( 'NONE', #8729, #11132, #8527, .T. ) ;
#1196 = AXIS2_PLACEMENT_3D ( 'NONE', #2619, #4610, #1638 ) ;
#1197 = ORIENTED_EDGE ( 'NONE', *, *, #9838, .T. ) ;
#1198 = ORIENTED_EDGE ( 'NONE', *, *, #1665, .T. ) ;
#1199 = ORIENTED_EDGE ( 'NONE', *, *, #5324, .F. ) ;
#1200 = ORIENTED_EDGE ( 'NONE', *, *, #2352, .F. ) ;
#1201 = CARTESIAN_POINT ( 'NONE',  ( -18.00000000000002842, 30.00000000000000000, 4.336808689942017736E-16 ) ) ;
#1202 = DIRECTION ( 'NONE',  ( 0.000000000000000000, 1.000000000000000000, 0.000000000000000000 ) ) ;
#1203 = EDGE_LOOP ( 'NONE', ( #10273, #6208, #1198, #629 ) ) ;
#1204 = DIRECTION ( 'NONE',  ( -0.000000000000000000, -1.000000000000000000, -0.000000000000000000 ) ) ;
#1205 = CIRCLE ( 'NONE', #11288, 9.999999999999998224 ) ;
#1206 = VERTEX_POINT ( 'NONE', #2693 ) ;
#1207 = CYLINDRICAL_SURFACE ( 'NONE', #10349, 2.800000000000003819 ) ;
#1208 = B_SPLINE_CURVE_WITH_KNOTS ( 'NONE', 3,
 ( #8974, #4082, #8009, #36, #1248 ),
 .UNSPECIFIED., .F., .F.,
 ( 4, 1, 4 ),
 ( 0.000000000000000000, 0.002309401076758506657, 0.004618802153517013315 ),
 .UNSPECIFIED. ) ;
#1209 = ADVANCED_FACE ( 'NONE', ( #7694 ), #6611, .T. ) ;
#1210 = DIRECTION ( 'NONE',  ( 0.000000000000000000, 0.9749279121818227312, 0.2225209339563182231 ) ) ;
#1211 = ADVANCED_FACE ( 'NONE', ( #1703 ), #9542, .T. ) ;
#1212 = CIRCLE ( 'NONE', #9019, 2.149999999999985256 ) ;
#1213 = AXIS2_PLACEMENT_3D ( 'NONE', #2855, #6705, #6830 ) ;
#1214 = DIRECTION ( 'NONE',  ( 1.031682152609352680E-29, 1.000000000000000000, -1.498801083243958569E-15 ) ) ;
#1215 = EDGE_LOOP ( 'NONE', ( #8140, #5838, #6921, #7199 ) ) ;
#1216 = AXIS2_PLACEMENT_3D ( 'NONE', #4875, #3912, #11772 ) ;
#1217 = CARTESIAN_POINT ( 'NONE',  ( 9.999999999999998224, 30.00000000000000000, -6.123233995736765296E-16 ) ) ;
#1218 = ORIENTED_EDGE ( 'NONE', *, *, #5875, .F. ) ;
#1219 = CYLINDRICAL_SURFACE ( 'NONE', #8884, 6.499000000000010324 ) ;
#1220 = CARTESIAN_POINT ( 'NONE',  ( 0.000000000000000000, -1.773042676681341856, 3.469446951953614189E-15 ) ) ;
#1221 = CIRCLE ( 'NONE', #10053, 7.400000000000011902 ) ;
#1222 = DIRECTION ( 'NONE',  ( -1.000000000000000000, 1.010728034814421376E-30, 1.090846720500930387E-30 ) ) ;
#1223 = CARTESIAN_POINT ( 'NONE',  ( 11.00000000000003020, 30.00000000000000000, 5.000000000000004441 ) ) ;
#1224 = EDGE_CURVE ( 'NONE', #5846, #3671, #9624, .T. ) ;
#1225 = CYLINDRICAL_SURFACE ( 'NONE', #5852, 2.499999999999998668 ) ;
#1226 = EDGE_CURVE ( 'NONE', #8657, #9126, #12529, .T. ) ;
#1227 = CARTESIAN_POINT ( 'NONE',  ( 19.99999999999999645, 0.000000000000000000, 0.000000000000000000 ) ) ;
#1228 = EDGE_CURVE ( 'NONE', #7688, #4329, #3065, .T. ) ;
#1229 = CARTESIAN_POINT ( 'NONE',  ( 0.000000000000000000, -2.401522331692820256, -6.999477872697425163 ) ) ;
#1230 = CIRCLE ( 'NONE', #8434, 6.499000000000006771 ) ;
#1231 = AXIS2_PLACEMENT_3D ( 'NONE', #5096, #3432, #5345 ) ;
#1232 = CARTESIAN_POINT ( 'NONE',  ( 11.00000000000001599, -12.49999999999999645, 3.994800001834461867E-31 ) ) ;
#1233 =( NAMED_UNIT ( * ) PLANE_ANGLE_UNIT ( ) SI_UNIT ( $, .RADIAN. ) );
#1234 = ADVANCED_FACE ( 'NONE', ( #11881 ), #3830, .T. ) ;
#1235 = EDGE_LOOP ( 'NONE', ( #8347, #1122, #10045, #7560 ) ) ;
#1236 = CARTESIAN_POINT ( 'NONE',  ( -31.74999999999995026, 2.449293598294707893E-16, -2.000000000000018208 ) ) ;
#1237 = DIRECTION ( 'NONE',  ( -3.260214209858708648E-30, -0.5000000000000012212, -0.8660254037844380415 ) ) ;
#1238 = AXIS2_PLACEMENT_3D ( 'NONE', #92, #33, #10841 ) ;
#1239 = CYLINDRICAL_SURFACE ( 'NONE', #2419, 14.99999999999998757 ) ;
#1240 = CARTESIAN_POINT ( 'NONE',  ( 15.00000000000003375, 30.00000000000001776, -4.000000000000008882 ) ) ;
#1241 = ORIENTED_EDGE ( 'NONE', *, *, #4147, .F. ) ;
#1242 = CARTESIAN_POINT ( 'NONE',  ( -11.83215956619923226, -30.00000000000000000, -2.000000000000000888 ) ) ;
#1243 = EDGE_CURVE ( 'NONE', #10380, #10576, #4983, .T. ) ;
#1244 = DIRECTION ( 'NONE',  ( -1.000000000000000000, 0.000000000000000000, 0.000000000000000000 ) ) ;
#1245 = EDGE_CURVE ( 'NONE', #6857, #5859, #1205, .T. ) ;
#1246 = DIRECTION ( 'NONE',  ( -1.000000000000000000, 1.010728034814421376E-30, 1.090846720500930387E-30 ) ) ;
#1247 = ORIENTED_EDGE ( 'NONE', *, *, #7927, .T. ) ;
#1248 = CARTESIAN_POINT ( 'NONE',  ( -4.000000000000012434, 2.309401076758501592, -3.433295621305395340 ) ) ;
#1249 = ORIENTED_EDGE ( 'NONE', *, *, #5103, .F. ) ;
#1250 = ORIENTED_EDGE ( 'NONE', *, *, #9318, .T. ) ;
#1251 = CARTESIAN_POINT ( 'NONE',  ( 40.00000000000000000, 39.34792583643766051, -14.91347054209569301 ) ) ;
#1252 = ORIENTED_EDGE ( 'NONE', *, *, #11293, .F. ) ;
#1253 = CYLINDRICAL_SURFACE ( 'NONE', #10328, 2.499999999999998668 ) ;
#1254 = ORIENTED_EDGE ( 'NONE', *, *, #1536, .F. ) ;
#1255 = PRESENTATION_STYLE_ASSIGNMENT (( #6281 ) ) ;
#1256 = CARTESIAN_POINT ( 'NONE',  ( 19.99999999999999645, 3.238809497145207494, 5.634457741540175313 ) ) ;
#1257 = CARTESIAN_POINT ( 'NONE',  ( 27.00000000000001421, 39.49790820824818383, -24.06186359251418594 ) ) ;
#1258 = DIRECTION ( 'NONE',  ( 1.000000000000000000, 1.081682119347366321E-16, -6.938893903907228378E-17 ) ) ;
#1259 = ADVANCED_FACE ( 'NONE', ( #4856 ), #6861, .F. ) ;
#1260 = ORIENTED_EDGE ( 'NONE', *, *, #7203, .T. ) ;
#1261 = VERTEX_POINT ( 'NONE', #7934 ) ;
#1262 = EDGE_CURVE ( 'NONE', #1632, #10195, #8192, .T. ) ;
#1263 = VERTEX_POINT ( 'NONE', #4073 ) ;
#1264 = ORIENTED_EDGE ( 'NONE', *, *, #7163, .F. ) ;
#1265 = CIRCLE ( 'NONE', #10096, 3.500000000000000000 ) ;
#1266 = DIRECTION ( 'NONE',  ( -1.000000000000000000, 1.010728034814421376E-30, 1.090846720500930387E-30 ) ) ;
#1267 = ADVANCED_FACE ( 'NONE', ( #85 ), #10767, .T. ) ;
#1268 = VECTOR ( 'NONE', #3945, 1000.000000000000000 ) ;
#1269 = CARTESIAN_POINT ( 'NONE',  ( 4.000000000000001776, 0.8378280264232703667, -3.220590601395643127 ) ) ;
#1270 = ORIENTED_EDGE ( 'NONE', *, *, #5502, .T. ) ;
#1271 = CARTESIAN_POINT ( 'NONE',  ( -2.499999999999965805, -3.438830781974908945E-14, -5.000000000000011546 ) ) ;
#1272 = VERTEX_POINT ( 'NONE', #2084 ) ;
#1273 = CARTESIAN_POINT ( 'NONE',  ( 19.99999999999999645, -0.9522442067291300161, 6.508557431545700211 ) ) ;
#1274 = CARTESIAN_POINT ( 'NONE',  ( 2.712762565639559309, -3.052587955997608127, -3.430618716626636200 ) ) ;
#1275 = EDGE_CURVE ( 'NONE', #10532, #8740, #9012, .T. ) ;
#1276 = FACE_OUTER_BOUND ( 'NONE', #3409, .T. ) ;
#1277 = ORIENTED_EDGE ( 'NONE', *, *, #10967, .F. ) ;
#1278 = DIRECTION ( 'NONE',  ( 1.000000000000000000, -1.010728034814421376E-30, -1.090846720500930387E-30 ) ) ;
#1279 = VERTEX_POINT ( 'NONE', #1952 ) ;
#1280 = DIRECTION ( 'NONE',  ( -1.000000000000000000, 0.000000000000000000, 0.000000000000000000 ) ) ;
#1281 = CIRCLE ( 'NONE', #11371, 7.400000000000011902 ) ;
#1282 = EDGE_CURVE ( 'NONE', #11062, #11320, #6003, .T. ) ;
#1283 = DIRECTION ( 'NONE',  ( -0.000000000000000000, -1.000000000000000000, -0.000000000000000000 ) ) ;
#1284 = AXIS2_PLACEMENT_3D ( 'NONE', #1858, #12691, #3862 ) ;
#1285 = EDGE_CURVE ( 'NONE', #8536, #5702, #860, .T. ) ;
#1286 = CARTESIAN_POINT ( 'NONE',  ( -15.00000000000000000, 2.465190328815661892E-29, 20.00000000000007461 ) ) ;
#1287 = ADVANCED_FACE ( 'NONE', ( #4920 ), #8781, .F. ) ;
#1288 = CARTESIAN_POINT ( 'NONE',  ( 14.00000000000000000, -13.00000000000000000, 0.000000000000000000 ) ) ;
#1289 = CARTESIAN_POINT ( 'NONE',  ( 40.00000000000006395, 1.290960574571364216E-15, -20.00000000000000000 ) ) ;
#1290 = CIRCLE ( 'NONE', #3170, 7.400000000000009237 ) ;
#1291 = CARTESIAN_POINT ( 'NONE',  ( 2.000000000000001776, -0.8865213383406727043, 1.535500000000009191 ) ) ;
#1292 = AXIS2_PLACEMENT_3D ( 'NONE', #3598, #12546, #5457 ) ;
#1293 = FACE_OUTER_BOUND ( 'NONE', #6936, .T. ) ;
#1294 = DIRECTION ( 'NONE',  ( -1.000000000000000000, -1.848892746611742259E-31, 1.154721252774410589E-34 ) ) ;
#1295 = VECTOR ( 'NONE', #3707, 1000.000000000000000 ) ;
#1296 = ADVANCED_FACE ( 'NONE', ( #7818 ), #3952, .T. ) ;
#1297 = EDGE_LOOP ( 'NONE', ( #2561, #7768, #10724, #11579 ) ) ;
#1298 = DIRECTION ( 'NONE',  ( 1.000000000000000000, 0.000000000000000000, 0.000000000000000000 ) ) ;
#1299 = FACE_OUTER_BOUND ( 'NONE', #4604, .T. ) ;
#1300 = B_SPLINE_CURVE_WITH_KNOTS ( 'NONE', 3,
 ( #1871, #3628, #6587, #9582, #4651, #5549 ),
 .UNSPECIFIED., .F., .F.,
 ( 4, 2, 4 ),
 ( -3.640115492409309580E-06, 0.0002066546034003389619, 0.0004169493222930872466 ),
 .UNSPECIFIED. ) ;
#1301 = CARTESIAN_POINT ( 'NONE',  ( 19.99999999999999645, -0.9522442067291300161, 6.508557431545700211 ) ) ;
#1302 = CARTESIAN_POINT ( 'NONE',  ( 19.99999999999997868, -2.385831757338501724, -6.045230171438906730 ) ) ;
#1303 = DIRECTION ( 'NONE',  ( 1.000000000000000000, 0.000000000000000000, 0.000000000000000000 ) ) ;
#1304 = CARTESIAN_POINT ( 'NONE',  ( 18.00000000000000355, 49.63999999999998636, -5.000000000000002665 ) ) ;
#1305 = EDGE_CURVE ( 'NONE', #12032, #2862, #9921, .T. ) ;
#1306 = CIRCLE ( 'NONE', #1525, 2.800000000000004263 ) ;
#1307 = APPLICATION_CONTEXT ( 'automotive_design' ) ;
#1308 = ORIENTED_EDGE ( 'NONE', *, *, #6615, .T. ) ;
#1309 = CARTESIAN_POINT ( 'NONE',  ( -30.00000000000000000, 0.000000000000000000, 2.000000000000001776 ) ) ;
#1310 = ORIENTED_EDGE ( 'NONE', *, *, #10574, .T. ) ;
#1311 = ORIENTED_EDGE ( 'NONE', *, *, #2045, .F. ) ;
#1312 = ITEM_DEFINED_TRANSFORMATION ( 'NONE', 'NONE', #11256,  #12422 ) ;
#1313 = ORIENTED_EDGE ( 'NONE', *, *, #6753, .F. ) ;
#1314 = EDGE_CURVE ( 'NONE', #2160, #10794, #1409, .T. ) ;
#1315 = AXIS2_PLACEMENT_3D ( 'NONE', #7370, #11292, #6400 ) ;
#1316 = CYLINDRICAL_SURFACE ( 'NONE', #4301, 7.400000000000010125 ) ;
#1317 = DIRECTION ( 'NONE',  ( 0.000000000000000000, -0.000000000000000000, -1.000000000000000000 ) ) ;
#1318 = ADVANCED_FACE ( 'NONE', ( #3131 ), #9024, .T. ) ;
#1319 = DIRECTION ( 'NONE',  ( 0.000000000000000000, 0.000000000000000000, 1.000000000000000000 ) ) ;
#1320 = PLANE ( 'NONE',  #6991 ) ;
#1321 = DIRECTION ( 'NONE',  ( 0.000000000000000000, 0.000000000000000000, -1.000000000000000000 ) ) ;
#1322 = CARTESIAN_POINT ( 'NONE',  ( 40.00000000000000000, 39.34792583643766051, -19.21347054209566352 ) ) ;
#1323 = DIRECTION ( 'NONE',  ( -3.437775699846489820E-17, -0.2951046417778627751, -0.9554649393887560960 ) ) ;
#1324 = EDGE_LOOP ( 'NONE', ( #1443, #12016, #2086, #5636 ) ) ;
#1325 = AXIS2_PLACEMENT_3D ( 'NONE', #1099, #911, #1880 ) ;
#1326 = AXIS2_PLACEMENT_3D ( 'NONE', #3544, #11648, #9502 ) ;
#1327 = VERTEX_POINT ( 'NONE', #2151 ) ;
#1328 = ORIENTED_EDGE ( 'NONE', *, *, #2045, .T. ) ;
#1329 = ORIENTED_EDGE ( 'NONE', *, *, #3041, .F. ) ;
#1330 = CARTESIAN_POINT ( 'NONE',  ( -10.00000000000000178, 0.000000000000000000, 0.000000000000000000 ) ) ;
#1331 = CARTESIAN_POINT ( 'NONE',  ( -1.390230914382133642, -4.043987460488810193, -3.502507215260537432 ) ) ;
#1332 = EDGE_LOOP ( 'NONE', ( #921, #250, #4664, #1712 ) ) ;
#1333 = LINE ( 'NONE', #5084, #4298 ) ;
#1334 = ORIENTED_EDGE ( 'NONE', *, *, #10118, .F. ) ;
#1335 = AXIS2_PLACEMENT_3D ( 'NONE', #7600, #3928, #1865 ) ;
#1336 = AXIS2_PLACEMENT_3D ( 'NONE', #3651, #3590, #11505 ) ;
#1337 = FACE_OUTER_BOUND ( 'NONE', #10473, .T. ) ;
#1338 = CARTESIAN_POINT ( 'NONE',  ( 0.000000000000000000, 4.862606272033057841, -3.745885042887454830 ) ) ;
#1339 = ADVANCED_FACE ( 'NONE', ( #6072 ), #10961, .T. ) ;
#1340 = CYLINDRICAL_SURFACE ( 'NONE', #12047, 10.00000000000000000 ) ;
#1341 = DIRECTION ( 'NONE',  ( -1.000000000000000000, 1.010728034814421376E-30, 1.090846720500930387E-30 ) ) ;
#1342 = ORIENTED_EDGE ( 'NONE', *, *, #9256, .T. ) ;
#1343 = EDGE_LOOP ( 'NONE', ( #979, #8656, #191, #6990, #9068 ) ) ;
#1344 = VECTOR ( 'NONE', #7617, 1000.000000000000000 ) ;
#1345 = CARTESIAN_POINT ( 'NONE',  ( 9.999999999999998224, 5.025702764809090617, 5.431603052487417038 ) ) ;
#1346 = DIRECTION ( 'NONE',  ( 0.000000000000000000, 0.000000000000000000, 1.000000000000000000 ) ) ;
#1347 = CARTESIAN_POINT ( 'NONE',  ( 19.99999999999997868, -2.099089055167727480, -6.233932467347804263 ) ) ;
#1348 = CARTESIAN_POINT ( 'NONE',  ( 40.00000000000000711, 10.63631887905126128, -9.927230231572499619 ) ) ;
#1349 = EDGE_CURVE ( 'NONE', #3794, #7169, #6770, .T. ) ;
#1350 = AXIS2_PLACEMENT_3D ( 'NONE', #10220, #2335, #1415 ) ;
#1351 = LINE ( 'NONE', #8252, #5877 ) ;
#1352 = CARTESIAN_POINT ( 'NONE',  ( 19.99999999999997868, 4.177097350749889415, -6.108343287861160320 ) ) ;
#1353 = ADVANCED_FACE ( 'NONE', ( #4624 ), #6691, .T. ) ;
#1354 = ORIENTED_EDGE ( 'NONE', *, *, #5714, .F. ) ;
#1355 = FACE_OUTER_BOUND ( 'NONE', #587, .T. ) ;
#1356 = EDGE_CURVE ( 'NONE', #2130, #6863, #7172, .T. ) ;
#1357 = FACE_OUTER_BOUND ( 'NONE', #4922, .T. ) ;
#1358 =( NAMED_UNIT ( * ) PLANE_ANGLE_UNIT ( ) SI_UNIT ( $, .RADIAN. ) );
#1359 = AXIS2_PLACEMENT_3D ( 'NONE', #6417, #10457, #8529 ) ;
#1360 = AXIS2_PLACEMENT_3D ( 'NONE', #1573, #12281, #5629 ) ;
#1361 = ORIENTED_EDGE ( 'NONE', *, *, #8700, .T. ) ;
#1362 = DIRECTION ( 'NONE',  ( 0.000000000000000000, 0.000000000000000000, -1.000000000000000000 ) ) ;
#1363 = DIRECTION ( 'NONE',  ( -1.000000000000000000, 1.010728034814421376E-30, 1.090846720500930387E-30 ) ) ;
#1364 = DIRECTION ( 'NONE',  ( -1.000000000000000000, 1.010728034814421376E-30, 1.090846720500930387E-30 ) ) ;
#1365 = CARTESIAN_POINT ( 'NONE',  ( 0.000000000000000000, 3.681899619563855808, -5.450844343808915582 ) ) ;
#1366 = CARTESIAN_POINT ( 'NONE',  ( 19.99999999999999645, -6.453973581750233279, -0.7636923504069568214 ) ) ;
#1367 = CIRCLE ( 'NONE', #11874, 2.800000000000003819 ) ;
#1368 = CARTESIAN_POINT ( 'NONE',  ( -30.00000000000000000, 19.99999999999999645, 2.000000000000003109 ) ) ;
#1369 = AXIS2_PLACEMENT_3D ( 'NONE', #11425, #2605, #7863 ) ;
#1370 = EDGE_CURVE ( 'NONE', #1182, #3532, #383, .T. ) ;
#1371 = FILL_AREA_STYLE ('',( #11235 ) ) ;
#1372 = ORIENTED_EDGE ( 'NONE', *, *, #11676, .T. ) ;
#1373 = PLANE ( 'NONE',  #10921 ) ;
#1374 = VERTEX_POINT ( 'NONE', #627 ) ;
#1375 = ORIENTED_EDGE ( 'NONE', *, *, #3001, .T. ) ;
#1376 = CONTEXT_DEPENDENT_SHAPE_REPRESENTATION ( #3553, #3899 ) ;
#1377 = SHAPE_REPRESENTATION ( 'Serrated Eccentric Cam Pawl', ( #12422 ), #2062 ) ;
#1378 = EDGE_LOOP ( 'NONE', ( #7121, #8465, #1600, #2100 ) ) ;
#1379 = ORIENTED_EDGE ( 'NONE', *, *, #1046, .F. ) ;
#1380 = CARTESIAN_POINT ( 'NONE',  ( -0.6448876103708466312, -4.246476118072349593, -0.2256878752776683428 ) ) ;
#1381 = AXIS2_PLACEMENT_3D ( 'NONE', #1005, #11646, #2965 ) ;
#1382 = CARTESIAN_POINT ( 'NONE',  ( 19.99999999999997868, 3.908107171477257058, -5.192658214849914522 ) ) ;
#1383 = CARTESIAN_POINT ( 'NONE',  ( 33.00000000000001421, 48.04086878529346194, 39.26975893117280947 ) ) ;
#1384 = DIRECTION ( 'NONE',  ( -0.000000000000000000, -1.000000000000000000, -0.000000000000000000 ) ) ;
#1385 = CARTESIAN_POINT ( 'NONE',  ( -27.85000000000000497, 2.632990618166801840E-16, 3.477184903947654954E-15 ) ) ;
#1386 = ORIENTED_EDGE ( 'NONE', *, *, #3946, .F. ) ;
#1387 = CARTESIAN_POINT ( 'NONE',  ( 19.99999999999999645, 0.000000000000000000, 0.000000000000000000 ) ) ;
#1388 = ADVANCED_FACE ( 'NONE', ( #6497 ), #180, .T. ) ;
#1389 = CYLINDRICAL_SURFACE ( 'NONE', #10685, 2.800000000000003819 ) ;
#1390 = ORIENTED_EDGE ( 'NONE', *, *, #11204, .T. ) ;
#1391 = ADVANCED_FACE ( 'NONE', ( #9429 ), #10451, .T. ) ;
#1392 = ORIENTED_EDGE ( 'NONE', *, *, #4468, .T. ) ;
#1393 = VERTEX_POINT ( 'NONE', #12553 ) ;
#1394 = EDGE_CURVE ( 'NONE', #8136, #2021, #2508, .T. ) ;
#1395 = ORIENTED_EDGE ( 'NONE', *, *, #11820, .T. ) ;
#1396 = FACE_OUTER_BOUND ( 'NONE', #8792, .T. ) ;
#1397 = VERTEX_POINT ( 'NONE', #3726 ) ;
#1398 = EDGE_CURVE ( 'NONE', #302, #815, #12426, .T. ) ;
#1399 = DIRECTION ( 'NONE',  ( -1.000000000000000000, 1.010728034814421376E-30, 1.090846720500930387E-30 ) ) ;
#1400 = VERTEX_POINT ( 'NONE', #11521 ) ;
#1401 = DIRECTION ( 'NONE',  ( 1.000000000000000000, -1.010728034814421376E-30, -1.090846720500930387E-30 ) ) ;
#1402 = DIRECTION ( 'NONE',  ( 1.000000000000000000, 5.916456789157575403E-31, -1.224646799147352714E-16 ) ) ;
#1403 = CIRCLE ( 'NONE', #10259, 6.000000000000013323 ) ;
#1404 = CARTESIAN_POINT ( 'NONE',  ( -27.85000000000000853, 2.632990618166797895E-16, 2.185182530847200403E-15 ) ) ;
#1405 = LINE ( 'NONE', #6114, #6788 ) ;
#1406 = ORIENTED_EDGE ( 'NONE', *, *, #852, .F. ) ;
#1407 = VERTEX_POINT ( 'NONE', #5459 ) ;
#1408 = CARTESIAN_POINT ( 'NONE',  ( 19.99999999999999645, -4.621065432155107011, 4.569765340993028779 ) ) ;
#1409 = CIRCLE ( 'NONE', #3880, 2.499999999999992006 ) ;
#1410 = DIRECTION ( 'NONE',  ( 1.000000000000000000, 1.081682119347366321E-16, -6.938893903907228378E-17 ) ) ;
#1411 = CARTESIAN_POINT ( 'NONE',  ( 0.000000000000000000, 1.052479792859144947, -6.413211932068313637 ) ) ;
#1412 = EDGE_CURVE ( 'NONE', #1057, #7720, #9213, .T. ) ;
#1413 = AXIS2_PLACEMENT_3D ( 'NONE', #283, #3270, #3142 ) ;
#1414 = AXIS2_PLACEMENT_3D ( 'NONE', #436, #9498, #8356 ) ;
#1415 = DIRECTION ( 'NONE',  ( 0.000000000000000000, 0.4338837391175525693, 0.9009688679024219216 ) ) ;
#1416 = CARTESIAN_POINT ( 'NONE',  ( 3.999999999999996447, 0.000000000000000000, 0.000000000000000000 ) ) ;
#1417 = CIRCLE ( 'NONE', #8620, 4.000000000000008882 ) ;
#1418 = CARTESIAN_POINT ( 'NONE',  ( 40.00000000000006395, 1.290960574571364216E-15, -20.00000000000000000 ) ) ;
#1419 = EDGE_LOOP ( 'NONE', ( #3925, #6074, #4357, #7931, #7137 ) ) ;
#1420 = CARTESIAN_POINT ( 'NONE',  ( 19.99999999999999645, -0.8135880386783197471, 6.527339685683405612 ) ) ;
#1421 = DIRECTION ( 'NONE',  ( -1.000000000000000000, -1.848892746611742259E-31, 1.154721252774410589E-34 ) ) ;
#1422 = EDGE_CURVE ( 'NONE', #3731, #12527, #3078, .T. ) ;
#1423 = CIRCLE ( 'NONE', #9627, 0.2000000000000000944 ) ;
#1424 = AXIS2_PLACEMENT_3D ( 'NONE', #12463, #7493, #4722 ) ;
#1425 = VECTOR ( 'NONE', #10437, 1000.000000000000000 ) ;
#1426 = AXIS2_PLACEMENT_3D ( 'NONE', #9293, #1384, #294 ) ;
#1427 = VERTEX_POINT ( 'NONE', #7520 ) ;
#1428 = DIRECTION ( 'NONE',  ( 0.000000000000000000, 1.000000000000000000, 0.000000000000000000 ) ) ;
#1429 = CARTESIAN_POINT ( 'NONE',  ( 19.99999999999999645, 0.2252065540229667429, 6.573992004634855668 ) ) ;
#1430 = DIRECTION ( 'NONE',  ( 0.000000000000000000, 0.000000000000000000, 1.000000000000000000 ) ) ;
#1431 = PLANE ( 'NONE',  #6524 ) ;
#1432 = DIRECTION ( 'NONE',  ( -1.000000000000000000, 1.010728034814421376E-30, 1.090846720500930387E-30 ) ) ;
#1433 = AXIS2_PLACEMENT_3D ( 'NONE', #8756, #64, #3989 ) ;
#1434 = AXIS2_PLACEMENT_3D ( 'NONE', #9786, #915, #4065 ) ;
#1435 = CIRCLE ( 'NONE', #8641, 4.499999999999999112 ) ;
#1436 = DIRECTION ( 'NONE',  ( -1.000000000000000000, 1.010728034814421376E-30, 1.090846720500930387E-30 ) ) ;
#1437 =( NAMED_UNIT ( * ) PLANE_ANGLE_UNIT ( ) SI_UNIT ( $, .RADIAN. ) );
#1438 = ORIENTED_EDGE ( 'NONE', *, *, #11480, .F. ) ;
#1439 = DIRECTION ( 'NONE',  ( 1.000000000000000000, 1.031065855027150586E-29, 2.218671295934092550E-30 ) ) ;
#1440 = ORIENTED_EDGE ( 'NONE', *, *, #12668, .F. ) ;
#1441 = ORIENTED_EDGE ( 'NONE', *, *, #1913, .F. ) ;
#1442 = MECHANICAL_DESIGN_GEOMETRIC_PRESENTATION_REPRESENTATION (  '', ( #12570 ), #6396 ) ;
#1443 = ORIENTED_EDGE ( 'NONE', *, *, #8327, .F. ) ;
#1444 = CIRCLE ( 'NONE', #11915, 9.999999999999998224 ) ;
#1445 = CARTESIAN_POINT ( 'NONE',  ( -10.00000000000000178, 0.000000000000000000, 0.000000000000000000 ) ) ;
#1446 = EDGE_CURVE ( 'NONE', #2582, #9681, #4705, .T. ) ;
#1447 = DIRECTION ( 'NONE',  ( -1.000000000000000000, 1.010728034814421376E-30, 1.090846720500930387E-30 ) ) ;
#1448 = ADVANCED_FACE ( 'NONE', ( #566 ), #1782, .T. ) ;
#1449 = CYLINDRICAL_SURFACE ( 'NONE', #6515, 49.99999999999995026 ) ;
#1451 = EDGE_CURVE ( 'NONE', #6667, #11644, #7648, .T. ) ;
#1450 = DIRECTION ( 'NONE',  ( -0.000000000000000000, -1.000000000000000000, -0.000000000000000000 ) ) ;
#1452 = CARTESIAN_POINT ( 'NONE',  ( -17.00000000000000000, 0.000000000000000000, 20.00000000000007461 ) ) ;
#1453 = EDGE_LOOP ( 'NONE', ( #9220, #3978, #10581, #435 ) ) ;
#1454 = CARTESIAN_POINT ( 'NONE',  ( 9.999999999999994671, -6.969736844459671232, -2.486517307195214244 ) ) ;
#1455 = MECHANICAL_DESIGN_GEOMETRIC_PRESENTATION_REPRESENTATION (  '', ( #2072 ), #11342 ) ;
#1456 = DIRECTION ( 'NONE',  ( 0.000000000000000000, 0.000000000000000000, -1.000000000000000000 ) ) ;
#1457 = ORIENTED_EDGE ( 'NONE', *, *, #8568, .F. ) ;
#1458 = VERTEX_POINT ( 'NONE', #3664 ) ;
#1459 = VERTEX_POINT ( 'NONE', #8418 ) ;
#1460 = EDGE_LOOP ( 'NONE', ( #11682, #3932, #985, #10990 ) ) ;
#1461 = LINE ( 'NONE', #10078, #6448 ) ;
#1462 = LINE ( 'NONE', #3417, #2826 ) ;
#1463 = VERTEX_POINT ( 'NONE', #7578 ) ;
#1464 = FACE_BOUND ( 'NONE', #5052, .T. ) ;
#1465 = AXIS2_PLACEMENT_3D ( 'NONE', #9991, #11040, #11890 ) ;
#1466 = VERTEX_POINT ( 'NONE', #4497 ) ;
#1467 = CARTESIAN_POINT ( 'NONE',  ( -9.000000000000000000, 49.63999999999998636, -7.000000000000000888 ) ) ;
#1468 = DIRECTION ( 'NONE',  ( 0.000000000000000000, 0.000000000000000000, 1.000000000000000000 ) ) ;
#1469 = FACE_OUTER_BOUND ( 'NONE', #12351, .T. ) ;
#1470 = AXIS2_PLACEMENT_3D ( 'NONE', #2203, #6124, #10032 ) ;
#1471 = LINE ( 'NONE', #3610, #7618 ) ;
#1472 = EDGE_CURVE ( 'NONE', #11132, #938, #6627, .T. ) ;
#1473 = ORIENTED_EDGE ( 'NONE', *, *, #1716, .F. ) ;
#1474 = ORIENTED_EDGE ( 'NONE', *, *, #3146, .T. ) ;
#1475 = DIRECTION ( 'NONE',  ( 0.000000000000000000, 0.000000000000000000, 1.000000000000000000 ) ) ;
#1476 =( NAMED_UNIT ( * ) PLANE_ANGLE_UNIT ( ) SI_UNIT ( $, .RADIAN. ) );
#1477 = EDGE_CURVE ( 'NONE', #4665, #9359, #3885, .T. ) ;
#1478 = CARTESIAN_POINT ( 'NONE',  ( 19.99999999999999645, 0.000000000000000000, 0.000000000000000000 ) ) ;
#1479 = EDGE_CURVE ( 'NONE', #6979, #2021, #10668, .T. ) ;
#1480 = AXIS2_PLACEMENT_3D ( 'NONE', #10434, #3686, #5610 ) ;
#1481 = ORIENTED_EDGE ( 'NONE', *, *, #5409, .F. ) ;
#1482 = CARTESIAN_POINT ( 'NONE',  ( 4.204115023516783012, -1.660442669500226565, -3.602151381774563177 ) ) ;
#1483 = CARTESIAN_POINT ( 'NONE',  ( 19.99999999999999645, 0.000000000000000000, 0.000000000000000000 ) ) ;
#1484 = DIRECTION ( 'NONE',  ( -1.000000000000000000, 1.010728034814421376E-30, 1.090846720500930387E-30 ) ) ;
#1485 = ORIENTED_EDGE ( 'NONE', *, *, #7308, .T. ) ;
#1486 = CARTESIAN_POINT ( 'NONE',  ( 0.5449313310647116992, 4.304185902836938915, -3.316620875263519341 ) ) ;
#1487 = VECTOR ( 'NONE', #10109, 1000.000000000000000 ) ;
#1488 = DIRECTION ( 'NONE',  ( -1.000000000000000000, 1.010728034814421376E-30, 1.090846720500930387E-30 ) ) ;
#1489 = CIRCLE ( 'NONE', #8063, 2.800000000000003375 ) ;
#1490 = DIRECTION ( 'NONE',  ( 0.000000000000000000, 0.000000000000000000, 1.000000000000000000 ) ) ;
#1491 = ORIENTED_EDGE ( 'NONE', *, *, #10519, .F. ) ;
#1492 = DIRECTION ( 'NONE',  ( -1.000000000000000000, 1.010728034814421376E-30, 1.090846720500930387E-30 ) ) ;
#1493 = LINE ( 'NONE', #3326, #11599 ) ;
#1494 = AXIS2_PLACEMENT_3D ( 'NONE', #11116, #5067, #2302 ) ;
#1495 = DIRECTION ( 'NONE',  ( 2.187388225841179596E-16, -0.9997704357740726522, -0.02142605311579142552 ) ) ;
#1496 = CARTESIAN_POINT ( 'NONE',  ( 0.000000000000000000, 4.862606272033057841, -3.745885042887454830 ) ) ;
#1497 = DIRECTION ( 'NONE',  ( 1.000000000000000000, -1.010728034814421376E-30, -1.090846720500930387E-30 ) ) ;
#1498 = AXIS2_PLACEMENT_3D ( 'NONE', #11593, #2721, #9508 ) ;
#1499 = CARTESIAN_POINT ( 'NONE',  ( 20.00000000000000000, 21.12780530657007461, -5.807015647486883481 ) ) ;
#1500 = EDGE_CURVE ( 'NONE', #3716, #5057, #2889, .T. ) ;
#1501 = CARTESIAN_POINT ( 'NONE',  ( 2.000000000000001776, 0.8865213383406657099, 1.535500000000022958 ) ) ;
#1502 = ORIENTED_EDGE ( 'NONE', *, *, #10839, .F. ) ;
#1503 = CARTESIAN_POINT ( 'NONE',  ( 11.00000000000003375, -6.123233995736749519E-16, 20.00000000000003553 ) ) ;
#1504 = ORIENTED_EDGE ( 'NONE', *, *, #3812, .T. ) ;
#1505 = VECTOR ( 'NONE', #12469, 1000.000000000000114 ) ;
#1506 = CONTEXT_DEPENDENT_SHAPE_REPRESENTATION ( #7007, #3253 ) ;
#1507 = ORIENTED_EDGE ( 'NONE', *, *, #12147, .T. ) ;
#1508 = VERTEX_POINT ( 'NONE', #12741 ) ;
#1509 = CARTESIAN_POINT ( 'NONE',  ( -45.00000000000001421, 19.99999999999999645, 3.443468848353431668E-15 ) ) ;
#1510 = FILL_AREA_STYLE ('',( #7502 ) ) ;
#1511 = DIRECTION ( 'NONE',  ( -1.224646799147352714E-16, -1.177425296209236909E-30, -1.000000000000000000 ) ) ;
#1512 = DIRECTION ( 'NONE',  ( 0.000000000000000000, 0.000000000000000000, 1.000000000000000000 ) ) ;
#1513 = ORIENTED_EDGE ( 'NONE', *, *, #8524, .F. ) ;
#1514 = CYLINDRICAL_SURFACE ( 'NONE', #12658, 2.800000000000003819 ) ;
#1515 = AXIS2_PLACEMENT_3D ( 'NONE', #11359, #2411, #589 ) ;
#1516 = DIRECTION ( 'NONE',  ( -1.000000000000000000, 1.010728034814421376E-30, 1.090846720500930387E-30 ) ) ;
#1517 = EDGE_LOOP ( 'NONE', ( #10586, #238, #7027, #9677, #2521, #5666, #4792, #7574 ) ) ;
#1518 = ORIENTED_EDGE ( 'NONE', *, *, #4952, .T. ) ;
#1519 = ADVANCED_FACE ( 'NONE', ( #11896 ), #9936, .T. ) ;
#1520 = DIRECTION ( 'NONE',  ( 0.000000000000000000, 0.000000000000000000, -1.000000000000000000 ) ) ;
#1521 = ORIENTED_EDGE ( 'NONE', *, *, #1893, .T. ) ;
#1522 = EDGE_CURVE ( 'NONE', #1090, #7272, #12705, .T. ) ;
#1523 = ORIENTED_EDGE ( 'NONE', *, *, #4552, .F. ) ;
#1524 = VECTOR ( 'NONE', #6266, 1000.000000000000000 ) ;
#1525 = AXIS2_PLACEMENT_3D ( 'NONE', #1273, #3171, #1150 ) ;
#1526 = VERTEX_POINT ( 'NONE', #10851 ) ;
#1527 = CARTESIAN_POINT ( 'NONE',  ( 14.00000000000000000, -30.00000000000000000, 0.000000000000000000 ) ) ;
#1528 = DIRECTION ( 'NONE',  ( -1.000000000000000000, 1.010728034814421376E-30, 1.090846720500930387E-30 ) ) ;
#1529 = EDGE_LOOP ( 'NONE', ( #9834, #5911, #8287, #3014, #1342 ) ) ;
#1530 = LINE ( 'NONE', #6436, #9724 ) ;
#1531 = DIRECTION ( 'NONE',  ( 1.000000000000000000, 1.849040895279789448E-31, -6.938893903907224680E-17 ) ) ;
#1532 = CIRCLE ( 'NONE', #9136, 14.99999999999998934 ) ;
#1533 = LINE ( 'NONE', #693, #11840 ) ;
#1534 = CARTESIAN_POINT ( 'NONE',  ( 0.000000000000000000, 0.000000000000000000, 0.000000000000000000 ) ) ;
#1535 = EDGE_LOOP ( 'NONE', ( #8025, #1673, #2551, #10246 ) ) ;
#1536 = EDGE_CURVE ( 'NONE', #4933, #5862, #5134, .T. ) ;
#1537 = ORIENTED_EDGE ( 'NONE', *, *, #8644, .T. ) ;
#1538 = DIRECTION ( 'NONE',  ( 1.000000000000000000, 0.000000000000000000, 0.000000000000000000 ) ) ;
#1539 = VECTOR ( 'NONE', #5857, 1000.000000000000000 ) ;
#1540 =( NAMED_UNIT ( * ) SI_UNIT ( $, .STERADIAN. ) SOLID_ANGLE_UNIT ( ) );
#1541 = CIRCLE ( 'NONE', #12254, 2.000000000000003553 ) ;
#1542 = CARTESIAN_POINT ( 'NONE',  ( 9.000000000000031974, 12.50000000000000000, 5.000000000000004441 ) ) ;
#1543 = CARTESIAN_POINT ( 'NONE',  ( -0.3208286057739651032, 4.433571671609682241, -0.3503314178412564317 ) ) ;
#1544 = CARTESIAN_POINT ( 'NONE',  ( 4.000000000000001776, -1.700175430507322449, -3.320327275037637804 ) ) ;
#1545 = CARTESIAN_POINT ( 'NONE',  ( 19.99999999999999645, -6.182645281642508372, 2.245659411033100294 ) ) ;
#1546 = VECTOR ( 'NONE', #10772, 1000.000000000000000 ) ;
#1547 = VECTOR ( 'NONE', #10508, 1000.000000000000000 ) ;
#1548 = FACE_OUTER_BOUND ( 'NONE', #5567, .T. ) ;
#1549 = EDGE_LOOP ( 'NONE', ( #9983, #8678 ) ) ;
#1550 = DIRECTION ( 'NONE',  ( -1.000000000000000000, 1.010728034814421376E-30, 1.090846720500930387E-30 ) ) ;
#1551 = EDGE_CURVE ( 'NONE', #10108, #10778, #3849, .T. ) ;
#1552 = LINE ( 'NONE', #8256, #6421 ) ;
#1553 = EDGE_CURVE ( 'NONE', #11498, #10609, #5066, .T. ) ;
#1554 =( NAMED_UNIT ( * ) PLANE_ANGLE_UNIT ( ) SI_UNIT ( $, .RADIAN. ) );
#1555 = DIRECTION ( 'NONE',  ( 1.000000000000000000, 1.081682119347366197E-16, -6.938893903907228378E-17 ) ) ;
#1556 = EDGE_LOOP ( 'NONE', ( #9726, #8104, #3428, #4027, #5974 ) ) ;
#1557 = AXIS2_PLACEMENT_3D ( 'NONE', #2137, #6252, #4257 ) ;
#1558 = CARTESIAN_POINT ( 'NONE',  ( 9.000000000000031974, 12.50000000000000000, -6.000000000000017764 ) ) ;
#1559 = EDGE_CURVE ( 'NONE', #3892, #1466, #1622, .T. ) ;
#1560 = CARTESIAN_POINT ( 'NONE',  ( 20.00000000000000355, 8.611173066148735344, -18.09125363591105540 ) ) ;
#1561 = CARTESIAN_POINT ( 'NONE',  ( -15.00000000000000711, -30.00000000000000000, 25.00000000000007105 ) ) ;
#1562 = CYLINDRICAL_SURFACE ( 'NONE', #4873, 6.000000000000000000 ) ;
#1563 = CYLINDRICAL_SURFACE ( 'NONE', #12684, 5.000000000000000888 ) ;
#1564 = CARTESIAN_POINT ( 'NONE',  ( 3.349226789952651107, 2.685125164760722605, -0.2236248678334721574 ) ) ;
#1565 =( LENGTH_UNIT ( ) NAMED_UNIT ( * ) SI_UNIT ( .MILLI., .METRE. ) );
#1566 = CONICAL_SURFACE ( 'NONE', #8574, 4.000000000000000000, 0.8911886515913786111 ) ;
#1567 = AXIS2_PLACEMENT_3D ( 'NONE', #7065, #2171, #7130 ) ;
#1568 = LINE ( 'NONE', #9162, #6405 ) ;
#1569 = ORIENTED_EDGE ( 'NONE', *, *, #8920, .T. ) ;
#1570 = ORIENTED_EDGE ( 'NONE', *, *, #5694, .F. ) ;
#1571 = ORIENTED_EDGE ( 'NONE', *, *, #9670, .F. ) ;
#1572 = CARTESIAN_POINT ( 'NONE',  ( 19.99999999999999645, 0.000000000000000000, 0.000000000000000000 ) ) ;
#1573 = CARTESIAN_POINT ( 'NONE',  ( 0.000000000000000000, -3.055252325922224621, 5.825248672282130613 ) ) ;
#1574 = CARTESIAN_POINT ( 'NONE',  ( 28.61000000000001009, 3.580469254416129843E-15, 2.000000000000003553 ) ) ;
#1575 = AXIS2_PLACEMENT_3D ( 'NONE', #1288, #10948, #10100 ) ;
#1576 = DIRECTION ( 'NONE',  ( 0.000000000000000000, -1.000000000000000000, 0.000000000000000000 ) ) ;
#1577 = VERTEX_POINT ( 'NONE', #1907 ) ;
#1578 = VECTOR ( 'NONE', #6610, 1000.000000000000000 ) ;
#1579 = CYLINDRICAL_SURFACE ( 'NONE', #6904, 6.499000000000010324 ) ;
#1580 = CARTESIAN_POINT ( 'NONE',  ( 11.17157287525379772, 12.99999999999999822, -2.828427124746177856 ) ) ;
#1581 = ORIENTED_EDGE ( 'NONE', *, *, #5569, .T. ) ;
#1582 = VERTEX_POINT ( 'NONE', #1846 ) ;
#1583 = DIRECTION ( 'NONE',  ( -1.000000000000000000, 0.000000000000000000, 0.000000000000000000 ) ) ;
#1584 = VERTEX_POINT ( 'NONE', #3083 ) ;
#1585 = PRODUCT_DEFINITION_FORMATION_WITH_SPECIFIED_SOURCE ( 'ANY', '', #8328, .NOT_KNOWN. ) ;
#1586 = EDGE_LOOP ( 'NONE', ( #3626, #12343, #10983, #4232 ) ) ;
#1587 = CIRCLE ( 'NONE', #5906, 3.500000000000003997 ) ;
#1588 = VECTOR ( 'NONE', #11611, 999.9999999999998863 ) ;
#1589 = DIRECTION ( 'NONE',  ( -1.081682119347366197E-16, 1.000000000000000000, 0.000000000000000000 ) ) ;
#1590 = ORIENTED_EDGE ( 'NONE', *, *, #6258, .T. ) ;
#1591 = DIRECTION ( 'NONE',  ( 0.000000000000000000, 0.1785568947986369281, -0.9839295885986296675 ) ) ;
#1592 = FACE_OUTER_BOUND ( 'NONE', #11349, .T. ) ;
#1593 = EDGE_LOOP ( 'NONE', ( #10858, #8430 ) ) ;
#1594 = CARTESIAN_POINT ( 'NONE',  ( -40.00000000000000000, 19.99999999999999645, 2.000000000000003109 ) ) ;
#1595 = EDGE_CURVE ( 'NONE', #1400, #5017, #4510, .T. ) ;
#1596 = DIRECTION ( 'NONE',  ( -1.257247067695985813E-30, 0.9749279121818227312, 0.2225209339563182509 ) ) ;
#1597 = VECTOR ( 'NONE', #10603, 1000.000000000000000 ) ;
#1598 = DIRECTION ( 'NONE',  ( -1.000000000000000000, 1.010728034814421376E-30, 1.090846720500930387E-30 ) ) ;
#1599 = CARTESIAN_POINT ( 'NONE',  ( 40.00000000000000711, 22.22477142302764364, -7.338293953734280173 ) ) ;
#1600 = ORIENTED_EDGE ( 'NONE', *, *, #6359, .F. ) ;
#1601 = ORIENTED_EDGE ( 'NONE', *, *, #5372, .T. ) ;
#1602 = DIRECTION ( 'NONE',  ( 0.000000000000000000, 0.000000000000000000, 1.000000000000000000 ) ) ;
#1603 = DIRECTION ( 'NONE',  ( 6.982962677686266711E-15, 0.000000000000000000, -1.000000000000000000 ) ) ;
#1604 = EDGE_LOOP ( 'NONE', ( #1991, #6241, #1590, #2296, #8881, #12609, #6350, #8005 ) ) ;
#1605 = DIRECTION ( 'NONE',  ( -1.000000000000000000, 1.010728034814421376E-30, 1.090846720500930387E-30 ) ) ;
#1606 = DIRECTION ( 'NONE',  ( 1.000000000000000000, -6.162975822039154730E-33, -4.563833282352349791E-17 ) ) ;
#1607 = EDGE_CURVE ( 'NONE', #3905, #2770, #8981, .T. ) ;
#1608 = EDGE_CURVE ( 'NONE', #4761, #363, #2464, .T. ) ;
#1609 = CARTESIAN_POINT ( 'NONE',  ( -2.727116801252319662E-30, 5.510332127717284397E-15, -2.499999999999999556 ) ) ;
#1610 = CARTESIAN_POINT ( 'NONE',  ( 1.734723475976807094E-14, -3.469446951953614189E-15, -4.000000000000010658 ) ) ;
#1611 = VERTEX_POINT ( 'NONE', #9810 ) ;
#1612 = AXIS2_PLACEMENT_3D ( 'NONE', #11456, #8542, #2573 ) ;
#1613 = DIRECTION ( 'NONE',  ( 0.000000000000000000, 0.000000000000000000, 1.000000000000000000 ) ) ;
#1614 = CARTESIAN_POINT ( 'NONE',  ( 15.00000000000003375, 12.50000000000000000, -4.062508476441825628E-31 ) ) ;
#1615 = SHAPE_REPRESENTATION_RELATIONSHIP ( 'NONE' , 'NONE' ,  #8378, #2668 ) ;
#1616 = CARTESIAN_POINT ( 'NONE',  ( 4.000000000000017764, -1.539600717839020527, -3.300726591567066492 ) ) ;
#1617 = AXIS2_PLACEMENT_3D ( 'NONE', #11073, #11142, #1520 ) ;
#1618 = VERTEX_POINT ( 'NONE', #163 ) ;
#1619 = CARTESIAN_POINT ( 'NONE',  ( 0.000000000000000000, 5.895746314278409450, 2.916892913127012488 ) ) ;
#1620 = FACE_OUTER_BOUND ( 'NONE', #6017, .T. ) ;
#1621 = PRODUCT_DEFINITION_SHAPE ( 'NONE', 'NONE',  #12763 ) ;
#1622 = CIRCLE ( 'NONE', #5741, 7.400000000000009237 ) ;
#1623 = CARTESIAN_POINT ( 'NONE',  ( 0.000000000000000000, 0.000000000000000000, 0.000000000000000000 ) ) ;
#1624 = DIRECTION ( 'NONE',  ( 0.000000000000000000, 0.000000000000000000, 1.000000000000000000 ) ) ;
#1625 = FACE_OUTER_BOUND ( 'NONE', #12477, .T. ) ;
#1626 = CARTESIAN_POINT ( 'NONE',  ( 3.679171394226029790, 2.494631558665822535, -0.3503314178412420543 ) ) ;
#1627 = CARTESIAN_POINT ( 'NONE',  ( 19.99999999999999645, -5.774092856145738750, 2.982759240804856660 ) ) ;
#1628 = AXIS2_PLACEMENT_3D ( 'NONE', #7984, #7866, #2997 ) ;
#1629 = AXIS2_PLACEMENT_3D ( 'NONE', #12368, #1722, #8543 ) ;
#1630 = EDGE_CURVE ( 'NONE', #6277, #6857, #876, .T. ) ;
#1631 = DIRECTION ( 'NONE',  ( -1.000000000000000000, 1.010728034814421376E-30, 1.090846720500930387E-30 ) ) ;
#1632 = VERTEX_POINT ( 'NONE', #1001 ) ;
#1633 = ORIENTED_EDGE ( 'NONE', *, *, #12507, .T. ) ;
#1634 = ORIENTED_EDGE ( 'NONE', *, *, #6345, .F. ) ;
#1635 = CYLINDRICAL_SURFACE ( 'NONE', #2337, 7.400000000000010125 ) ;
#1636 = AXIS2_PLACEMENT_3D ( 'NONE', #7668, #2982, #8815 ) ;
#1637 = DIRECTION ( 'NONE',  ( 0.000000000000000000, 1.000000000000000000, 0.000000000000000000 ) ) ;
#1638 = DIRECTION ( 'NONE',  ( 1.140150527077241873E-30, 0.000000000000000000, -1.000000000000000000 ) ) ;
#1639 = AXIS2_PLACEMENT_3D ( 'NONE', #5607, #12637, #7605 ) ;
#1640 = CIRCLE ( 'NONE', #11928, 2.800000000000004263 ) ;
#1641 = EDGE_CURVE ( 'NONE', #3905, #1917, #6781, .T. ) ;
#1642 = CARTESIAN_POINT ( 'NONE',  ( 19.99999999999999645, 2.918117354836642363, 5.807029542149858337 ) ) ;
#1643 = ORIENTED_EDGE ( 'NONE', *, *, #454, .F. ) ;
#1644 = ADVANCED_FACE ( 'NONE', ( #7002 ), #6361, .T. ) ;
#1645 = CYLINDRICAL_SURFACE ( 'NONE', #11220, 3.500000000000003997 ) ;
#1646 = CYLINDRICAL_SURFACE ( 'NONE', #11537, 7.400000000000010125 ) ;
#1647 = ORIENTED_EDGE ( 'NONE', *, *, #5811, .T. ) ;
#1648 = EDGE_LOOP ( 'NONE', ( #4098, #11451, #3860, #9831 ) ) ;
#1649 = CARTESIAN_POINT ( 'NONE',  ( 9.999999999999998224, 0.2110513566294528187, -7.396989747516558467 ) ) ;
#1650 = EDGE_LOOP ( 'NONE', ( #4150, #4153, #284, #4995 ) ) ;
#1651 = AXIS2_PLACEMENT_3D ( 'NONE', #11186, #8281, #2434 ) ;
#1652 = ORIENTED_EDGE ( 'NONE', *, *, #9989, .F. ) ;
#1653 = CIRCLE ( 'NONE', #1617, 6.999999999999999112 ) ;
#1654 = CIRCLE ( 'NONE', #4737, 2.800000000000003819 ) ;
#1655 = SURFACE_SIDE_STYLE ('',( #4680 ) ) ;
#1656 = DIRECTION ( 'NONE',  ( 1.000000000000000000, 1.081682119347366197E-16, -6.938893903907228378E-17 ) ) ;
#1657 = ORIENTED_EDGE ( 'NONE', *, *, #6911, .F. ) ;
#1658 = CARTESIAN_POINT ( 'NONE',  ( 19.99999999999997868, 3.238809497145301197, -5.634457741540144227 ) ) ;
#1659 = LINE ( 'NONE', #5460, #10280 ) ;
#1660 = EDGE_CURVE ( 'NONE', #9362, #4951, #10461, .T. ) ;
#1661 = VERTEX_POINT ( 'NONE', #4939 ) ;
#1662 = CARTESIAN_POINT ( 'NONE',  ( -14.99999999999999289, 30.00000000000000000, 25.00000000000007105 ) ) ;
#1663 = DIRECTION ( 'NONE',  ( 1.000000000000000000, -0.000000000000000000, -0.000000000000000000 ) ) ;
#1664 = MANIFOLD_SOLID_BREP ( 'EndChamfer', #1069 ) ;
#1665 = EDGE_CURVE ( 'NONE', #8569, #4277, #1189, .T. ) ;
#1666 = FACE_OUTER_BOUND ( 'NONE', #11127, .T. ) ;
#1667 = ADVANCED_FACE ( 'NONE', ( #7835 ), #4159, .T. ) ;
#1668 = EDGE_LOOP ( 'NONE', ( #2219, #492, #3445, #8221, #7910 ) ) ;
#1669 = ORIENTED_EDGE ( 'NONE', *, *, #11869, .F. ) ;
#1670 = CARTESIAN_POINT ( 'NONE',  ( 14.00000000000000000, -30.00000000000000000, 0.000000000000000000 ) ) ;
#1671 = MECHANICAL_DESIGN_GEOMETRIC_PRESENTATION_REPRESENTATION (  '', ( #4964 ), #9261 ) ;
#1672 = DIRECTION ( 'NONE',  ( 6.982962677686266711E-15, 0.000000000000000000, -1.000000000000000000 ) ) ;
#1673 = ORIENTED_EDGE ( 'NONE', *, *, #5824, .F. ) ;
#1674 = DIRECTION ( 'NONE',  ( -1.000000000000000000, 1.010728034814421376E-30, 1.090846720500930387E-30 ) ) ;
#1675 = FACE_OUTER_BOUND ( 'NONE', #12675, .T. ) ;
#1676 = EDGE_CURVE ( 'NONE', #10778, #4568, #11050, .T. ) ;
#1677 = DIRECTION ( 'NONE',  ( -1.000000000000000000, -1.848892746611742259E-31, 1.154721252774410589E-34 ) ) ;
#1678 = AXIS2_PLACEMENT_3D ( 'NONE', #7119, #2227, #221 ) ;
#1679 = DIRECTION ( 'NONE',  ( 1.000000000000000000, -6.162975822039154730E-33, -4.563833282352349791E-17 ) ) ;
#1680 = EDGE_LOOP ( 'NONE', ( #10061, #10515, #602, #1018 ) ) ;
#1681 = CARTESIAN_POINT ( 'NONE',  ( 19.99999999999999645, 0.000000000000000000, 0.000000000000000000 ) ) ;
#1682 = LINE ( 'NONE', #4589, #9483 ) ;
#1683 = EDGE_CURVE ( 'NONE', #5519, #3706, #8079, .T. ) ;
#1684 = ADVANCED_FACE ( 'NONE', ( #3216 ), #1316, .T. ) ;
#1685 = CYLINDRICAL_SURFACE ( 'NONE', #3911, 2.800000000000003819 ) ;
#1686 = CIRCLE ( 'NONE', #45, 6.000000000000000888 ) ;
#1687 = DIRECTION ( 'NONE',  ( 0.000000000000000000, 0.000000000000000000, 1.000000000000000000 ) ) ;
#1688 = DIRECTION ( 'NONE',  ( -1.000000000000000000, -1.081682119347366444E-16, 5.551115123125780237E-17 ) ) ;
#1689 = FACE_OUTER_BOUND ( 'NONE', #9355, .T. ) ;
#1690 = DIRECTION ( 'NONE',  ( -1.000000000000000000, 1.010728034814421376E-30, 1.090846720500930387E-30 ) ) ;
#1691 = DIRECTION ( 'NONE',  ( -0.000000000000000000, -1.000000000000000000, -0.000000000000000000 ) ) ;
#1692 = DIRECTION ( 'NONE',  ( 1.000000000000000000, -1.010728034814421376E-30, -1.090846720500930387E-30 ) ) ;
#1693 = CARTESIAN_POINT ( 'NONE',  ( -15.00000000000000000, -20.00000000000000000, 14.15000000000002167 ) ) ;
#1694 = ORIENTED_EDGE ( 'NONE', *, *, #2030, .F. ) ;
#1695 = EDGE_CURVE ( 'NONE', #6900, #3787, #2674, .T. ) ;
#1696 = MANIFOLD_SOLID_BREP ( 'Extrude-Thin1', #2109 ) ;
#1697 = ORIENTED_EDGE ( 'NONE', *, *, #1717, .F. ) ;
#1698 = EDGE_LOOP ( 'NONE', ( #12167, #10076, #4423, #3828 ) ) ;
#1699 = AXIS2_PLACEMENT_3D ( 'NONE', #2942, #5880, #4917 ) ;
#1700 = CARTESIAN_POINT ( 'NONE',  ( 4.000000000000019540, -2.309401076758522464, -3.433295621305367806 ) ) ;
#1701 = AXIS2_PLACEMENT_3D ( 'NONE', #5779, #5011, #9759 ) ;
#1702 = CARTESIAN_POINT ( 'NONE',  ( -17.00000000000000000, 0.000000000000000000, 20.00000000000007461 ) ) ;
#1703 = FACE_OUTER_BOUND ( 'NONE', #1332, .T. ) ;
#1704 = CARTESIAN_POINT ( 'NONE',  ( 0.1999999999999987899, 0.000000000000000000, 0.000000000000000000 ) ) ;
#1705 = ORIENTED_EDGE ( 'NONE', *, *, #9638, .F. ) ;
#1706 = EDGE_CURVE ( 'NONE', #1045, #7990, #1417, .T. ) ;
#1707 = CARTESIAN_POINT ( 'NONE',  ( 27.00000000000001421, 81.84122341717352356, -27.68198508464163510 ) ) ;
#1708 = EDGE_CURVE ( 'NONE', #3334, #9611, #3336, .T. ) ;
#1709 = CARTESIAN_POINT ( 'NONE',  ( 0.000000000000000000, 0.000000000000000000, 0.000000000000000000 ) ) ;
#1710 = EDGE_LOOP ( 'NONE', ( #11981, #7930, #10266 ) ) ;
#1711 = VECTOR ( 'NONE', #12408, 1000.000000000000000 ) ;
#1712 = ORIENTED_EDGE ( 'NONE', *, *, #2405, .T. ) ;
#1713 = CARTESIAN_POINT ( 'NONE',  ( 0.000000000000000000, -5.362766118793872216, 3.671204237728608266 ) ) ;
#1714 = ORIENTED_EDGE ( 'NONE', *, *, #8066, .F. ) ;
#1715 = ORIENTED_EDGE ( 'NONE', *, *, #3433, .F. ) ;
#1716 = EDGE_CURVE ( 'NONE', #5117, #1836, #10245, .T. ) ;
#1717 = EDGE_CURVE ( 'NONE', #9801, #3793, #601, .T. ) ;
#1718 = CYLINDRICAL_SURFACE ( 'NONE', #6790, 2.800000000000003819 ) ;
#1719 = ORIENTED_EDGE ( 'NONE', *, *, #11169, .F. ) ;
#1720 = EDGE_CURVE ( 'NONE', #2523, #10664, #12109, .T. ) ;
#1721 = DIRECTION ( 'NONE',  ( 0.000000000000000000, 0.000000000000000000, 1.000000000000000000 ) ) ;
#1722 = DIRECTION ( 'NONE',  ( -1.000000000000000000, 1.010728034814421376E-30, 1.090846720500930387E-30 ) ) ;
#1723 = ORIENTED_EDGE ( 'NONE', *, *, #5620, .T. ) ;
#1724 = VECTOR ( 'NONE', #2011, 1000.000000000000000 ) ;
#1725 = CARTESIAN_POINT ( 'NONE',  ( 0.000000000000000000, 6.613766744932247477, 3.319350756342029474 ) ) ;
#1726 = ADVANCED_FACE ( 'NONE', ( #8797 ), #12739, .T. ) ;
#1727 = DIRECTION ( 'NONE',  ( 0.000000000000000000, 0.000000000000000000, -1.000000000000000000 ) ) ;
#1728 = UNCERTAINTY_MEASURE_WITH_UNIT (LENGTH_MEASURE( 1.000000000000000082E-05 ), #6656, 'distance_accuracy_value', 'NONE');
#1729 = ORIENTED_EDGE ( 'NONE', *, *, #8152, .T. ) ;
#1730 = AXIS2_PLACEMENT_3D ( 'NONE', #8509, #7743, #1080 ) ;
#1731 = ORIENTED_EDGE ( 'NONE', *, *, #1522, .T. ) ;
#1732 = APPLICATION_CONTEXT ( 'automotive_design' ) ;
#1733 = CYLINDRICAL_SURFACE ( 'NONE', #7269, 7.400000000000010125 ) ;
#1734 = VERTEX_POINT ( 'NONE', #11518 ) ;
#1735 = CARTESIAN_POINT ( 'NONE',  ( 40.00000000000000711, 12.07894703944102943, -21.64141622710139146 ) ) ;
#1736 = CIRCLE ( 'NONE', #9323, 2.800000000000002931 ) ;
#1737 = DIRECTION ( 'NONE',  ( 0.000000000000000000, 0.000000000000000000, -1.000000000000000000 ) ) ;
#1738 = DIRECTION ( 'NONE',  ( 0.000000000000000000, -1.530455820933490821E-32, 1.000000000000000000 ) ) ;
#1739 = ADVANCED_BREP_SHAPE_REPRESENTATION ( '', ( #5956, #12422 ), #20 ) ;
#1740 = DIRECTION ( 'NONE',  ( 0.000000000000000000, 0.000000000000000000, 1.000000000000000000 ) ) ;
#1741 = ORIENTED_EDGE ( 'NONE', *, *, #7200, .F. ) ;
#1742 = CARTESIAN_POINT ( 'NONE',  ( -2.000000000000008882, -3.464101615137750390, -8.673617379884035472E-15 ) ) ;
#1743 = AXIS2_PLACEMENT_3D ( 'NONE', #4385, #9515, #11278 ) ;
#1744 = ORIENTED_EDGE ( 'NONE', *, *, #3604, .T. ) ;
#1745 = AXIS2_PLACEMENT_3D ( 'NONE', #6437, #3358, #1468 ) ;
#1746 = DIRECTION ( 'NONE',  ( 0.000000000000000000, 0.000000000000000000, 1.000000000000000000 ) ) ;
#1747 = LINE ( 'NONE', #5613, #2900 ) ;
#1748 = CARTESIAN_POINT ( 'NONE',  ( -10.00000000000000178, 0.000000000000000000, 0.000000000000000000 ) ) ;
#1749 = EDGE_CURVE ( 'NONE', #3985, #10901, #874, .T. ) ;
#1750 = LINE ( 'NONE', #844, #10761 ) ;
#1752 = CARTESIAN_POINT ( 'NONE',  ( 19.99999999999999645, 0.000000000000000000, 0.000000000000000000 ) ) ;
#1751 = AXIS2_PLACEMENT_3D ( 'NONE', #634, #5467, #4438 ) ;
#1753 = DIRECTION ( 'NONE',  ( 0.000000000000000000, 0.000000000000000000, 1.000000000000000000 ) ) ;
#1754 = CIRCLE ( 'NONE', #4433, 24.99999999999998934 ) ;
#1755 = ADVANCED_FACE ( 'NONE', ( #939 ), #3662, .F. ) ;
#1756 = DIRECTION ( 'NONE',  ( 6.902532920683843663E-31, -0.9749279121818259508, 0.2225209339563040956 ) ) ;
#1757 = EDGE_CURVE ( 'NONE', #9234, #4686, #5709, .T. ) ;
#1758 = LINE ( 'NONE', #3575, #2566 ) ;
#1759 = DIRECTION ( 'NONE',  ( -1.000000000000000000, -1.031065855027150586E-29, 2.218671295934095703E-30 ) ) ;
#1760 = LINE ( 'NONE', #8775, #9472 ) ;
#1761 = ORIENTED_EDGE ( 'NONE', *, *, #646, .F. ) ;
#1762 = CIRCLE ( 'NONE', #117, 7.400000000000009237 ) ;
#1763 = VERTEX_POINT ( 'NONE', #11768 ) ;
#1764 = ORIENTED_EDGE ( 'NONE', *, *, #9514, .T. ) ;
#1765 = DIRECTION ( 'NONE',  ( -2.280301054154484185E-31, -0.5877852522924801315, 0.8090169943749423442 ) ) ;
#1766 = DIRECTION ( 'NONE',  ( -1.000000000000000000, -5.916456789157575403E-31, 1.577021341797098793E-16 ) ) ;
#1767 = CARTESIAN_POINT ( 'NONE',  ( 19.99999999999999645, 0.4528593230174772222, 7.386130139224198921 ) ) ;
#1768 = CARTESIAN_POINT ( 'NONE',  ( 0.000000000000000000, 6.146182963951696721, -2.112211157443803611 ) ) ;
#1769 = ORIENTED_EDGE ( 'NONE', *, *, #9334, .F. ) ;
#1770 = DIRECTION ( 'NONE',  ( 1.238279320584846685E-16, -0.9554649393887558739, 0.2951046417778634412 ) ) ;
#1771 = ADVANCED_FACE ( 'NONE', ( #809 ), #1905, .T. ) ;
#1772 = STYLED_ITEM ( 'NONE', ( #12365 ), #5705 ) ;
#1773 = CYLINDRICAL_SURFACE ( 'NONE', #8442, 7.400000000000010125 ) ;
#1774 = ORIENTED_EDGE ( 'NONE', *, *, #6435, .F. ) ;
#1775 = ORIENTED_EDGE ( 'NONE', *, *, #8895, .T. ) ;
#1776 = CARTESIAN_POINT ( 'NONE',  ( 20.00000000000000000, 10.63631887905125950, -9.927230231572497843 ) ) ;
#1777 = ORIENTED_EDGE ( 'NONE', *, *, #10672, .F. ) ;
#1778 = VERTEX_POINT ( 'NONE', #6875 ) ;
#1779 =( LENGTH_UNIT ( ) NAMED_UNIT ( * ) SI_UNIT ( .MILLI., .METRE. ) );
#1780 = CARTESIAN_POINT ( 'NONE',  ( -10.00000000000000178, 0.000000000000000000, 0.000000000000000000 ) ) ;
#1781 = ORIENTED_EDGE ( 'NONE', *, *, #2838, .T. ) ;
#1782 = CYLINDRICAL_SURFACE ( 'NONE', #3494, 2.800000000000003819 ) ;
#1783 = DIRECTION ( 'NONE',  ( -1.000000000000000000, 0.000000000000000000, 0.000000000000000000 ) ) ;
#1784 = ORIENTED_EDGE ( 'NONE', *, *, #6220, .F. ) ;
#1785 = CARTESIAN_POINT ( 'NONE',  ( 9.999999999999998224, 6.613766744932301656, -3.319350756341945985 ) ) ;
#1786 = CYLINDRICAL_SURFACE ( 'NONE', #8936, 2.800000000000003819 ) ;
#1787 = EDGE_CURVE ( 'NONE', #9004, #2431, #10718, .T. ) ;
#1788 = DIRECTION ( 'NONE',  ( 0.000000000000000000, 0.000000000000000000, 1.000000000000000000 ) ) ;
#1789 = EDGE_CURVE ( 'NONE', #5127, #3630, #7770, .T. ) ;
#1790 = AXIS2_PLACEMENT_3D ( 'NONE', #3328, #7245, #11163 ) ;
#1791 = AXIS2_PLACEMENT_3D ( 'NONE', #10565, #10692, #4781 ) ;
#1792 = VERTEX_POINT ( 'NONE', #7575 ) ;
#1793 = ORIENTED_EDGE ( 'NONE', *, *, #2345, .F. ) ;
#1794 = CARTESIAN_POINT ( 'NONE',  ( 2.000000000000001776, 1.773042676681341856, -3.469446951953614189E-15 ) ) ;
#1795 = EDGE_CURVE ( 'NONE', #1734, #9663, #11530, .T. ) ;
#1796 = CARTESIAN_POINT ( 'NONE',  ( 0.000000000000000000, 0.000000000000000000, 0.000000000000000000 ) ) ;
#1797 = ORIENTED_EDGE ( 'NONE', *, *, #2499, .F. ) ;
#1798 = CARTESIAN_POINT ( 'NONE',  ( -3.999999999999970690, -2.309401076758515359, -5.000000000000018652 ) ) ;
#1799 = CARTESIAN_POINT ( 'NONE',  ( 20.00000000000000000, 10.64574963035789601, -21.19875926443459591 ) ) ;
#1800 = AXIS2_PLACEMENT_3D ( 'NONE', #5396, #4500, #5649 ) ;
#1801 = EDGE_CURVE ( 'NONE', #4676, #3717, #5748, .T. ) ;
#1802 = ADVANCED_FACE ( 'NONE', ( #747 ), #7645, .T. ) ;
#1803 = CARTESIAN_POINT ( 'NONE',  ( 0.000000000000000000, 0.000000000000000000, 0.000000000000000000 ) ) ;
#1804 = LINE ( 'NONE', #5917, #5550 ) ;
#1805 = ORIENTED_EDGE ( 'NONE', *, *, #9881, .F. ) ;
#1806 = CARTESIAN_POINT ( 'NONE',  ( 0.000000000000000000, 6.018220532833807646, -2.453165835849195453 ) ) ;
#1807 = VERTEX_POINT ( 'NONE', #12615 ) ;
#1808 = LINE ( 'NONE', #10500, #12392 ) ;
#1809 = DIRECTION ( 'NONE',  ( -1.000000000000000000, 1.010728034814421376E-30, 1.090846720500930387E-30 ) ) ;
#1810 = CARTESIAN_POINT ( 'NONE',  ( 0.000000000000000000, -4.155687294075626426, 5.098857909653524700 ) ) ;
#1811 = DIRECTION ( 'NONE',  ( 0.000000000000000000, 0.000000000000000000, 1.000000000000000000 ) ) ;
#1812 = DIRECTION ( 'NONE',  ( 0.000000000000000000, 0.000000000000000000, 1.000000000000000000 ) ) ;
#1813 = DIRECTION ( 'NONE',  ( -1.000000000000000000, 1.010728034814421376E-30, 1.090846720500930387E-30 ) ) ;
#1814 = DIRECTION ( 'NONE',  ( 1.000000000000000000, 0.000000000000000000, 0.000000000000000000 ) ) ;
#1815 = DIRECTION ( 'NONE',  ( -1.000000000000000000, 1.010728034814421376E-30, 1.090846720500930387E-30 ) ) ;
#1816 = ADVANCED_FACE ( 'NONE', ( #3783 ), #1718, .T. ) ;
#1817 = DIRECTION ( 'NONE',  ( 0.000000000000000000, 0.000000000000000000, -1.000000000000000000 ) ) ;
#1818 = UNCERTAINTY_MEASURE_WITH_UNIT (LENGTH_MEASURE( 1.000000000000000082E-05 ), #8735, 'distance_accuracy_value', 'NONE');
#1819 = FACE_OUTER_BOUND ( 'NONE', #3970, .T. ) ;
#1820 = EDGE_CURVE ( 'NONE', #6210, #11779, #1021, .T. ) ;
#1821 = AXIS2_PLACEMENT_3D ( 'NONE', #212, #8058, #5111 ) ;
#1822 = VERTEX_POINT ( 'NONE', #10654 ) ;
#1823 = EDGE_LOOP ( 'NONE', ( #12079, #4616, #6876, #7646, #2549, #2027, #4556, #1218, #11515 ) ) ;
#1824 = CARTESIAN_POINT ( 'NONE',  ( 2.000000000000001776, -0.8865213383406691516, 1.535500000000002085 ) ) ;
#1825 =( LENGTH_UNIT ( ) NAMED_UNIT ( * ) SI_UNIT ( .MILLI., .METRE. ) );
#1826 = CARTESIAN_POINT ( 'NONE',  ( 0.1999999999999987899, 4.041334437186265510E-16, -3.300000000000017142 ) ) ;
#1827 = DIRECTION ( 'NONE',  ( 0.000000000000000000, 4.478906847412192569E-32, -1.000000000000000000 ) ) ;
#1828 = VERTEX_POINT ( 'NONE', #9680 ) ;
#1829 = DIRECTION ( 'NONE',  ( -7.025792437124625182E-30, -0.4999999999999992784, 0.8660254037844390407 ) ) ;
#1830 = AXIS2_PLACEMENT_3D ( 'NONE', #4258, #12127, #4322 ) ;
#1831 = AXIS2_PLACEMENT_3D ( 'NONE', #8871, #4958, #6761 ) ;
#1832 = SURFACE_SIDE_STYLE ('',( #9673 ) ) ;
#1833 = ORIENTED_EDGE ( 'NONE', *, *, #9129, .F. ) ;
#1834 = ORIENTED_EDGE ( 'NONE', *, *, #11321, .T. ) ;
#1835 = FACE_OUTER_BOUND ( 'NONE', #7253, .T. ) ;
#1836 = VERTEX_POINT ( 'NONE', #4809 ) ;
#1837 = ORIENTED_EDGE ( 'NONE', *, *, #11450, .F. ) ;
#1838 = EDGE_CURVE ( 'NONE', #4793, #2771, #197, .T. ) ;
#1839 = EDGE_CURVE ( 'NONE', #5204, #2655, #5643, .T. ) ;
#1840 = VECTOR ( 'NONE', #10679, 1000.000000000000000 ) ;
#1841 = CARTESIAN_POINT ( 'NONE',  ( 19.99999999999999645, -6.459281472512932609, -1.243290685169442966 ) ) ;
#1842 = EDGE_CURVE ( 'NONE', #7990, #8864, #4935, .T. ) ;
#1843 = VECTOR ( 'NONE', #8772, 1000.000000000000000 ) ;
#1844 = ORIENTED_EDGE ( 'NONE', *, *, #5034, .T. ) ;
#1845 = CIRCLE ( 'NONE', #9850, 6.499000000000008548 ) ;
#1846 = CARTESIAN_POINT ( 'NONE',  ( 2.000000000000001776, -0.8865213383406727043, 1.535500000000009191 ) ) ;
#1847 = EDGE_CURVE ( 'NONE', #7505, #11033, #6165, .T. ) ;
#1848 = LINE ( 'NONE', #10657, #1912 ) ;
#1849 = VERTEX_POINT ( 'NONE', #4219 ) ;
#1850 = AXIS2_PLACEMENT_3D ( 'NONE', #8562, #5785, #9765 ) ;
#1851 = LINE ( 'NONE', #1785, #10008 ) ;
#1852 = CARTESIAN_POINT ( 'NONE',  ( 15.00000000000003375, -29.99999999999998224, 9.742497179615118866E-31 ) ) ;
#1853 = VECTOR ( 'NONE', #6550, 1000.000000000000000 ) ;
#1854 = VECTOR ( 'NONE', #6775, 1000.000000000000000 ) ;
#1855 = ORIENTED_EDGE ( 'NONE', *, *, #1842, .T. ) ;
#1856 = ORIENTED_EDGE ( 'NONE', *, *, #4784, .T. ) ;
#1857 = ORIENTED_EDGE ( 'NONE', *, *, #3811, .F. ) ;
#1858 = CARTESIAN_POINT ( 'NONE',  ( 0.000000000000000000, 2.520781513113740324, -6.075668640744172677 ) ) ;
#1859 = EDGE_CURVE ( 'NONE', #7604, #11454, #8226, .T. ) ;
#1860 = EDGE_LOOP ( 'NONE', ( #689, #1241, #5697, #1744 ) ) ;
#1861 = CARTESIAN_POINT ( 'NONE',  ( 3.355112389629171243, -2.681727112203169838, -0.2256878752776775299 ) ) ;
#1862 = EDGE_LOOP ( 'NONE', ( #7189, #9790, #12181 ) ) ;
#1863 = DIRECTION ( 'NONE',  ( 0.000000000000000000, 0.5128992774059070170, -0.8584487936018656562 ) ) ;
#1864 = EDGE_CURVE ( 'NONE', #9310, #4937, #7061, .T. ) ;
#1865 = DIRECTION ( 'NONE',  ( -1.140150527077241873E-30, 0.000000000000000000, 1.000000000000000000 ) ) ;
#1866 = DIRECTION ( 'NONE',  ( 0.000000000000000000, 0.000000000000000000, -1.000000000000000000 ) ) ;
#1867 = EDGE_LOOP ( 'NONE', ( #3480, #9604, #3827, #3918 ) ) ;
#1869 = CARTESIAN_POINT ( 'NONE',  ( 40.00000000000000711, 14.86906044972264240, -7.469374795321334304 ) ) ;
#1868 = PRESENTATION_LAYER_ASSIGNMENT (  '', '', ( #7841 ) ) ;
#1870 = ORIENTED_EDGE ( 'NONE', *, *, #1720, .T. ) ;
#1871 = CARTESIAN_POINT ( 'NONE',  ( -4.211140560182161430, -2.431303136016561783, -3.745885042887451277 ) ) ;
#1872 =( NAMED_UNIT ( * ) SI_UNIT ( $, .STERADIAN. ) SOLID_ANGLE_UNIT ( ) );
#1873 = EDGE_CURVE ( 'NONE', #9471, #9760, #10978, .T. ) ;
#1874 = DIRECTION ( 'NONE',  ( 0.000000000000000000, -1.000000000000000000, 0.000000000000000000 ) ) ;
#1875 = DIRECTION ( 'NONE',  ( 1.000000000000000000, 0.000000000000000000, 0.000000000000000000 ) ) ;
#1876 = DIRECTION ( 'NONE',  ( 0.000000000000000000, 0.000000000000000000, 1.000000000000000000 ) ) ;
#1877 = AXIS2_PLACEMENT_3D ( 'NONE', #1503, #5243, #8267 ) ;
#1878 = FACE_OUTER_BOUND ( 'NONE', #1378, .T. ) ;
#1879 = CARTESIAN_POINT ( 'NONE',  ( 0.000000000000000000, -3.399584271718375739, 6.572885726945587592 ) ) ;
#1880 = DIRECTION ( 'NONE',  ( 0.000000000000000000, 0.000000000000000000, -1.000000000000000000 ) ) ;
#1881 = CARTESIAN_POINT ( 'NONE',  ( 19.99999999999997868, 6.321830586517952710, -1.817291089601262621 ) ) ;
#1882 =( LENGTH_UNIT ( ) NAMED_UNIT ( * ) SI_UNIT ( .MILLI., .METRE. ) );
#1883 = CIRCLE ( 'NONE', #6833, 6.499000000000008548 ) ;
#1884 = LINE ( 'NONE', #9470, #12385 ) ;
#1885 = AXIS2_PLACEMENT_3D ( 'NONE', #7237, #12196, #5357 ) ;
#1886 = ORIENTED_EDGE ( 'NONE', *, *, #6349, .T. ) ;
#1887 = ORIENTED_EDGE ( 'NONE', *, *, #3389, .T. ) ;
#1888 = CARTESIAN_POINT ( 'NONE',  ( 19.99999999999997868, 2.649444137877677186, -6.020675595748665287 ) ) ;
#1889 = CARTESIAN_POINT ( 'NONE',  ( 9.000000000000031974, -6.123233995736753463E-16, 20.00000000000003553 ) ) ;
#1890 = CARTESIAN_POINT ( 'NONE',  ( 14.00000000000000000, 30.00000000000000000, 0.000000000000000000 ) ) ;
#1891 = DIRECTION ( 'NONE',  ( -4.563833282352349791E-17, 0.000000000000000000, -1.000000000000000000 ) ) ;
#1892 = ORIENTED_EDGE ( 'NONE', *, *, #4957, .T. ) ;
#1893 = EDGE_CURVE ( 'NONE', #5416, #41, #1845, .T. ) ;
#1894 = CYLINDRICAL_SURFACE ( 'NONE', #3820, 2.000000000000003109 ) ;
#1895 = CIRCLE ( 'NONE', #2324, 2.149999999999992362 ) ;
#1896 = DIRECTION ( 'NONE',  ( -0.9396926207859138680, 5.234467192292534210E-33, -0.3420201433256536139 ) ) ;
#1897 = DIRECTION ( 'NONE',  ( -1.000000000000000000, 1.010728034814421376E-30, 1.090846720500930387E-30 ) ) ;
#1898 = ORIENTED_EDGE ( 'NONE', *, *, #1224, .T. ) ;
#1899 = ORIENTED_EDGE ( 'NONE', *, *, #578, .T. ) ;
#1900 = DIRECTION ( 'NONE',  ( -1.000000000000000000, 1.010728034814421376E-30, 1.090846720500930387E-30 ) ) ;
#1901 = VERTEX_POINT ( 'NONE', #9996 ) ;
#1902 = ORIENTED_EDGE ( 'NONE', *, *, #1349, .T. ) ;
#1903 = CIRCLE ( 'NONE', #669, 2.800000000000003819 ) ;
#1904 = AXIS2_PLACEMENT_3D ( 'NONE', #1014, #3921, #11906 ) ;
#1905 = CYLINDRICAL_SURFACE ( 'NONE', #11093, 2.800000000000003819 ) ;
#1906 = ORIENTED_EDGE ( 'NONE', *, *, #11800, .T. ) ;
#1907 = CARTESIAN_POINT ( 'NONE',  ( -15.00000000000003375, -30.00000000000000000, 3.000000000000029754 ) ) ;
#1908 = DIRECTION ( 'NONE',  ( 1.000867273499157327E-29, 0.8660254037844379305, -0.5000000000000012212 ) ) ;
#1909 = ORIENTED_EDGE ( 'NONE', *, *, #10219, .F. ) ;
#1910 = DIRECTION ( 'NONE',  ( 0.000000000000000000, -1.000000000000000000, 0.000000000000000000 ) ) ;
#1911 = DIRECTION ( 'NONE',  ( 3.260214209858707948E-30, 0.5000000000000011102, 0.8660254037844380415 ) ) ;
#1912 = VECTOR ( 'NONE', #6942, 1000.000000000000000 ) ;
#1913 = EDGE_CURVE ( 'NONE', #3292, #11603, #1187, .T. ) ;
#1914 = EDGE_CURVE ( 'NONE', #10811, #9165, #1640, .T. ) ;
#1915 = ORIENTED_EDGE ( 'NONE', *, *, #2093, .T. ) ;
#1916 = ORIENTED_EDGE ( 'NONE', *, *, #2991, .T. ) ;
#1917 = VERTEX_POINT ( 'NONE', #7123 ) ;
#1918 = DIRECTION ( 'NONE',  ( -1.848892746611746419E-31, -1.000000000000000000, 3.250006781153460502E-32 ) ) ;
#1919 = VECTOR ( 'NONE', #11565, 1000.000000000000000 ) ;
#1920 = ORIENTED_EDGE ( 'NONE', *, *, #3854, .F. ) ;
#1921 = CARTESIAN_POINT ( 'NONE',  ( 33.00000000000001421, 39.34792583643766761, -17.06347054209568270 ) ) ;
#1922 = ORIENTED_EDGE ( 'NONE', *, *, #7577, .F. ) ;
#1923 = DIRECTION ( 'NONE',  ( 0.000000000000000000, 0.000000000000000000, -1.000000000000000000 ) ) ;
#1924 = DIRECTION ( 'NONE',  ( -0.000000000000000000, -1.000000000000000000, -0.000000000000000000 ) ) ;
#1925 = AXIS2_PLACEMENT_3D ( 'NONE', #3817, #1401, #11266 ) ;
#1926 = LINE ( 'NONE', #7854, #1840 ) ;
#1927 = ORIENTED_EDGE ( 'NONE', *, *, #12089, .F. ) ;
#1928 = CYLINDRICAL_SURFACE ( 'NONE', #6172, 7.400000000000010125 ) ;
#1929 = ORIENTED_EDGE ( 'NONE', *, *, #5468, .F. ) ;
#1930 = CARTESIAN_POINT ( 'NONE',  ( 19.99999999999997868, 0.6915992404090851586, -6.462096524400249287 ) ) ;
#1931 = SURFACE_SIDE_STYLE ('',( #11015 ) ) ;
#1932 = AXIS2_PLACEMENT_3D ( 'NONE', #2950, #3012, #4989 ) ;
#1933 = CARTESIAN_POINT ( 'NONE',  ( 2.000000000000001776, 0.8865213383406657099, 1.535500000000022958 ) ) ;
#1934 = CARTESIAN_POINT ( 'NONE',  ( 34.00000000000000000, 0.000000000000000000, -1.734723475976807094E-14 ) ) ;
#1935 = DIRECTION ( 'NONE',  ( 0.000000000000000000, 0.000000000000000000, 1.000000000000000000 ) ) ;
#1936 = CARTESIAN_POINT ( 'NONE',  ( -35.00000000000006395, -19.99999999999999645, 2.168404344971008868E-15 ) ) ;
#1937 = LINE ( 'NONE', #10885, #2591 ) ;
#1938 = CIRCLE ( 'NONE', #2995, 2.500000000000000888 ) ;
#1939 = ADVANCED_FACE ( 'NONE', ( #6937 ), #4999, .T. ) ;
#1940 = VECTOR ( 'NONE', #5035, 1000.000000000000000 ) ;
#1941 = LINE ( 'NONE', #6914, #4924 ) ;
#1942 = EDGE_CURVE ( 'NONE', #5074, #303, #40, .T. ) ;
#1943 = PLANE ( 'NONE',  #2694 ) ;
#1944 = CARTESIAN_POINT ( 'NONE',  ( -3.999999999999994671, -2.309401076758511806, -0.4999999999999865663 ) ) ;
#1945 = ADVANCED_FACE ( 'NONE', ( #4026 ), #225, .F. ) ;
#1946 = AXIS2_PLACEMENT_3D ( 'NONE', #3484, #11269, #5334 ) ;
#1947 = EDGE_LOOP ( 'NONE', ( #8020, #6144, #3063, #8330 ) ) ;
#1948 = VECTOR ( 'NONE', #2107, 1000.000000000000000 ) ;
#1949 = ORIENTED_EDGE ( 'NONE', *, *, #11374, .T. ) ;
#1950 = CARTESIAN_POINT ( 'NONE',  ( 3.122502256758252770E-14, -4.618802153517027165, -3.433295621305388678 ) ) ;
#1951 = DIRECTION ( 'NONE',  ( -1.000000000000000000, 1.010728034814421376E-30, 1.090846720500930387E-30 ) ) ;
#1952 = CARTESIAN_POINT ( 'NONE',  ( 40.00000000000000711, 10.25912655421750230, -11.14847175327134110 ) ) ;
#1953 = CARTESIAN_POINT ( 'NONE',  ( -32.14999999999998437, 0.000000000000000000, 2.185182530847200403E-15 ) ) ;
#1954 = VERTEX_POINT ( 'NONE', #11894 ) ;
#1955 = DIRECTION ( 'NONE',  ( 0.000000000000000000, 0.000000000000000000, 1.000000000000000000 ) ) ;
#1956 = AXIS2_PLACEMENT_3D ( 'NONE', #704, #10495, #12187 ) ;
#1957 = CARTESIAN_POINT ( 'NONE',  ( 27.00000000000001421, 81.84122341717352356, -27.68198508464163510 ) ) ;
#1958 = DIRECTION ( 'NONE',  ( 0.000000000000000000, 1.177425296209236909E-30, 1.000000000000000000 ) ) ;
#1959 = ORIENTED_EDGE ( 'NONE', *, *, #8551, .T. ) ;
#1960 = AXIS2_PLACEMENT_3D ( 'NONE', #10965, #8263, #2155 ) ;
#1961 = VERTEX_POINT ( 'NONE', #4156 ) ;
#1962 = LINE ( 'NONE', #3904, #12124 ) ;
#1963 = ORIENTED_EDGE ( 'NONE', *, *, #11213, .F. ) ;
#1964 = B_SPLINE_CURVE_WITH_KNOTS ( 'NONE', 3,
 ( #11740, #10820, #7865, #8828, #16, #4003 ),
 .UNSPECIFIED., .F., .F.,
 ( 4, 2, 4 ),
 ( 0.003358874760055555794, 0.004541967308452096383, 0.005725059856848637406 ),
 .UNSPECIFIED. ) ;
#1965 = ORIENTED_EDGE ( 'NONE', *, *, #7963, .F. ) ;
#1966 = APPLICATION_PROTOCOL_DEFINITION ( 'draft international standard', 'automotive_design', 1998, #3061 ) ;
#1967 = CARTESIAN_POINT ( 'NONE',  ( -35.00000000000006395, -2.157041537713704155E-29, 2.000000000000003553 ) ) ;
#1968 = ORIENTED_EDGE ( 'NONE', *, *, #6206, .F. ) ;
#1969 = DIRECTION ( 'NONE',  ( -1.000000000000000000, 1.010728034814421376E-30, 1.090846720500930387E-30 ) ) ;
#1970 = CARTESIAN_POINT ( 'NONE',  ( 0.000000000000000000, 3.908107171477253505, -5.192658214849918075 ) ) ;
#1971 = EDGE_LOOP ( 'NONE', ( #7157, #9270, #9490, #4872 ) ) ;
#1972 = LINE ( 'NONE', #6944, #8795 ) ;
#1973 =( REPRESENTATION_RELATIONSHIP ('NONE','NONE', #10018, #8305 ) REPRESENTATION_RELATIONSHIP_WITH_TRANSFORMATION ( #2230 )SHAPE_REPRESENTATION_RELATIONSHIP( ) );
#1974 = DIRECTION ( 'NONE',  ( 0.000000000000000000, 5.551115123125776539E-17, 1.000000000000000000 ) ) ;
#1975 = ORIENTED_EDGE ( 'NONE', *, *, #12321, .T. ) ;
#1976 = ORIENTED_EDGE ( 'NONE', *, *, #4473, .F. ) ;
#1977 = ORIENTED_EDGE ( 'NONE', *, *, #6329, .F. ) ;
#1978 = AXIS2_PLACEMENT_3D ( 'NONE', #1452, #926, #10645 ) ;
#1979 = DIRECTION ( 'NONE',  ( -1.000000000000000000, 6.162975822039154730E-33, 4.563833282352349791E-17 ) ) ;
#1980 = VECTOR ( 'NONE', #7321, 1000.000000000000000 ) ;
#1981 = EDGE_LOOP ( 'NONE', ( #7314, #3852, #8670, #1856 ) ) ;
#1982 = DIRECTION ( 'NONE',  ( 0.000000000000000000, 0.000000000000000000, 1.000000000000000000 ) ) ;
#1983 = EDGE_LOOP ( 'NONE', ( #1087, #486, #3233, #4564 ) ) ;
#1984 = CIRCLE ( 'NONE', #6311, 2.149999999999985256 ) ;
#1985 = CIRCLE ( 'NONE', #1169, 7.400000000000011902 ) ;
#1986 = CARTESIAN_POINT ( 'NONE',  ( 32.99999999999999289, 39.34792583643766051, -14.91347054209568945 ) ) ;
#1987 = CARTESIAN_POINT ( 'NONE',  ( 0.000000000000000000, 0.000000000000000000, 0.000000000000000000 ) ) ;
#1988 = ORIENTED_EDGE ( 'NONE', *, *, #3075, .T. ) ;
#1989 = DIRECTION ( 'NONE',  ( -0.000000000000000000, -0.9883022714608525883, 0.1525077710325583313 ) ) ;
#1990 = PRODUCT_DEFINITION_CONTEXT ( 'detailed design', #7485, 'design' ) ;
#1991 = ORIENTED_EDGE ( 'NONE', *, *, #9650, .F. ) ;
#1992 = DIRECTION ( 'NONE',  ( 0.000000000000000000, 0.000000000000000000, 1.000000000000000000 ) ) ;
#1993 = EDGE_LOOP ( 'NONE', ( #10669, #10613, #8744, #5830 ) ) ;
#1994 =( NAMED_UNIT ( * ) SI_UNIT ( $, .STERADIAN. ) SOLID_ANGLE_UNIT ( ) );
#1995 = VECTOR ( 'NONE', #5411, 1000.000000000000000 ) ;
#1996 = CIRCLE ( 'NONE', #9193, 7.400000000000009237 ) ;
#1997 = ADVANCED_FACE ( 'NONE', ( #6997 ), #2099, .T. ) ;
#1998 = CARTESIAN_POINT ( 'NONE',  ( 19.99999999999999645, 5.956456411769392112, 2.790827096699012522 ) ) ;
#1999 = EDGE_CURVE ( 'NONE', #5702, #5083, #6986, .T. ) ;
#2000 = EDGE_CURVE ( 'NONE', #5523, #6000, #3096, .T. ) ;
#2001 = DIRECTION ( 'NONE',  ( 1.000000000000000000, -1.010728034814421376E-30, -1.090846720500930387E-30 ) ) ;
#2002 = CARTESIAN_POINT ( 'NONE',  ( 2.000000000000001776, -0.8865213383406727043, 1.535500000000009191 ) ) ;
#2003 = DIRECTION ( 'NONE',  ( -3.437775699846489820E-17, -0.2951046417778627751, -0.9554649393887560960 ) ) ;
#2004 = PLANE ( 'NONE',  #7497 ) ;
#2005 = EDGE_CURVE ( 'NONE', #3964, #1526, #10483, .T. ) ;
#2006 = DIRECTION ( 'NONE',  ( -1.000000000000000000, 1.010728034814421376E-30, 1.090846720500930387E-30 ) ) ;
#2007 = FACE_BOUND ( 'NONE', #4689, .T. ) ;
#2008 = DIRECTION ( 'NONE',  ( 1.000000000000000000, -1.010728034814421376E-30, -1.090846720500930387E-30 ) ) ;
#2009 = EDGE_LOOP ( 'NONE', ( #11304, #3949, #12355, #174 ) ) ;
#2010 = CARTESIAN_POINT ( 'NONE',  ( 19.99999999999999645, -3.055252325922228174, 5.825248672282130613 ) ) ;
#2011 = DIRECTION ( 'NONE',  ( 1.000000000000000000, 1.849040895279789448E-31, -6.938893903907224680E-17 ) ) ;
#2012 = FACE_OUTER_BOUND ( 'NONE', #573, .T. ) ;
#2013 = CARTESIAN_POINT ( 'NONE',  ( 9.999999999999998224, 3.975087478966649712, 6.241688836730239665 ) ) ;
#2014 = CARTESIAN_POINT ( 'NONE',  ( 0.000000000000000000, 0.000000000000000000, 0.000000000000000000 ) ) ;
#2015 = VERTEX_POINT ( 'NONE', #3214 ) ;
#2016 = CARTESIAN_POINT ( 'NONE',  ( 4.197393957002303999, 7.389034437926038210E-14, -3.503767560748934251 ) ) ;
#2017 = CARTESIAN_POINT ( 'NONE',  ( 0.1999999999999987899, 0.000000000000000000, 0.000000000000000000 ) ) ;
#2018 = EDGE_CURVE ( 'NONE', #93, #11435, #10677, .T. ) ;
#2019 = PRESENTATION_STYLE_ASSIGNMENT (( #6077 ) ) ;
#2020 = VERTEX_POINT ( 'NONE', #10849 ) ;
#2021 = VERTEX_POINT ( 'NONE', #1251 ) ;
#2022 = DIRECTION ( 'NONE',  ( 0.000000000000000000, 0.000000000000000000, 1.000000000000000000 ) ) ;
#2023 = ORIENTED_EDGE ( 'NONE', *, *, #11135, .F. ) ;
#2024 = ORIENTED_EDGE ( 'NONE', *, *, #4685, .T. ) ;
#2025 = PRODUCT_CONTEXT ( 'NONE', #2397, 'mechanical' ) ;
#2026 = DIRECTION ( 'NONE',  ( -3.437775699846489820E-17, -0.2951046417778627751, -0.9554649393887560960 ) ) ;
#2027 = ORIENTED_EDGE ( 'NONE', *, *, #11377, .T. ) ;
#2028 = EDGE_CURVE ( 'NONE', #2020, #2096, #6368, .T. ) ;
#2029 = SURFACE_STYLE_USAGE ( .BOTH. , #8858 ) ;
#2030 = EDGE_CURVE ( 'NONE', #3319, #2041, #1747, .T. ) ;
#2031 = DIRECTION ( 'NONE',  ( -1.000000000000000000, 1.010728034814421376E-30, 1.090846720500930387E-30 ) ) ;
#2032 = EDGE_LOOP ( 'NONE', ( #3642, #6100, #12638, #3784 ) ) ;
#2033 = VECTOR ( 'NONE', #5157, 1000.000000000000000 ) ;
#2034 = CIRCLE ( 'NONE', #1213, 6.499000000000009436 ) ;
#2035 = CYLINDRICAL_SURFACE ( 'NONE', #7555, 2.800000000000003819 ) ;
#2036 = DIRECTION ( 'NONE',  ( 0.000000000000000000, 0.000000000000000000, 1.000000000000000000 ) ) ;
#2037 = MECHANICAL_DESIGN_GEOMETRIC_PRESENTATION_REPRESENTATION (  '', ( #391 ), #6977 ) ;
#2038 = ORIENTED_EDGE ( 'NONE', *, *, #10834, .F. ) ;
#2039 = ORIENTED_EDGE ( 'NONE', *, *, #6604, .T. ) ;
#2040 = AXIS2_PLACEMENT_3D ( 'NONE', #645, #10362, #1740 ) ;
#2041 = VERTEX_POINT ( 'NONE', #5673 ) ;
#2042 = CIRCLE ( 'NONE', #6789, 6.000000000000000000 ) ;
#2043 = AXIS2_PLACEMENT_3D ( 'NONE', #8736, #12677, #11697 ) ;
#2044 = DIRECTION ( 'NONE',  ( 0.000000000000000000, 0.000000000000000000, -1.000000000000000000 ) ) ;
#2045 = EDGE_CURVE ( 'NONE', #6829, #742, #10054, .T. ) ;
#2046 = LINE ( 'NONE', #8931, #12274 ) ;
#2047 = VECTOR ( 'NONE', #3153, 1000.000000000000114 ) ;
#2048 = ORIENTED_EDGE ( 'NONE', *, *, #9917, .F. ) ;
#2049 = CARTESIAN_POINT ( 'NONE',  ( 20.00000000000000000, 11.10553687445042570, -10.07215277424222855 ) ) ;
#2050 = EDGE_LOOP ( 'NONE', ( #8866, #9247, #9932, #4731 ) ) ;
#2051 = EDGE_CURVE ( 'NONE', #7451, #12421, #7675, .T. ) ;
#2052 = AXIS2_PLACEMENT_3D ( 'NONE', #6837, #899, #1866 ) ;
#2053 = AXIS2_PLACEMENT_3D ( 'NONE', #5932, #5874, #18 ) ;
#2054 = VECTOR ( 'NONE', #969, 1000.000000000000000 ) ;
#2055 = EDGE_CURVE ( 'NONE', #7946, #5257, #4725, .T. ) ;
#2056 = LINE ( 'NONE', #5982, #6902 ) ;
#2057 = CARTESIAN_POINT ( 'NONE',  ( 9.757359312880696578, 30.00000000000000000, -4.242640687119267007 ) ) ;
#2058 = ORIENTED_EDGE ( 'NONE', *, *, #1412, .T. ) ;
#2059 = CARTESIAN_POINT ( 'NONE',  ( 9.714451465470119729E-14, -0.8865213383406727043, -1.535499999999998755 ) ) ;
#2060 = EDGE_LOOP ( 'NONE', ( #7767, #6994, #3073, #6097 ) ) ;
#2061 = DIRECTION ( 'NONE',  ( 1.140150527077241873E-30, 0.000000000000000000, -1.000000000000000000 ) ) ;
#2062 =( GEOMETRIC_REPRESENTATION_CONTEXT ( 3 ) GLOBAL_UNCERTAINTY_ASSIGNED_CONTEXT ( ( #5469 ) ) GLOBAL_UNIT_ASSIGNED_CONTEXT ( ( #2406, #6390, #11551 ) ) REPRESENTATION_CONTEXT ( 'NONE', 'WORKASPACE' ) );
#2063 = VECTOR ( 'NONE', #7763, 1000.000000000000000 ) ;
#2064 = PRESENTATION_STYLE_ASSIGNMENT (( #10877 ) ) ;
#2065 = VECTOR ( 'NONE', #7917, 1000.000000000000227 ) ;
#2066 = LINE ( 'NONE', #11735, #10 ) ;
#2067 = EDGE_CURVE ( 'NONE', #11719, #825, #10881, .T. ) ;
#2068 = FACE_OUTER_BOUND ( 'NONE', #2362, .T. ) ;
#2069 = CARTESIAN_POINT ( 'NONE',  ( 9.999999999999994671, -6.413745496774073906, -3.691052519622338490 ) ) ;
#2070 = CARTESIAN_POINT ( 'NONE',  ( 19.99999999999999645, -3.426907987218856810, 5.522074125465504579 ) ) ;
#2071 = DIRECTION ( 'NONE',  ( -1.000000000000000000, 0.000000000000000000, 0.000000000000000000 ) ) ;
#2072 = STYLED_ITEM ( 'NONE', ( #10216 ), #9258 ) ;
#2073 = LINE ( 'NONE', #5995, #4306 ) ;
#2074 = EDGE_CURVE ( 'NONE', #11856, #4356, #7599, .T. ) ;
#2075 = CARTESIAN_POINT ( 'NONE',  ( 20.00000000000000000, 15.24625277455639072, -6.248133273622503481 ) ) ;
#2076 = EDGE_CURVE ( 'NONE', #8334, #4606, #9637, .T. ) ;
#2077 = EDGE_CURVE ( 'NONE', #12721, #8586, #4865, .T. ) ;
#2078 = DIRECTION ( 'NONE',  ( -1.000000000000000000, 1.010728034814421376E-30, 1.090846720500930387E-30 ) ) ;
#2079 = COLOUR_RGB ( '', 0.72549020, 0.75294118, 0.79215686) ;
#2080 = ORIENTED_EDGE ( 'NONE', *, *, #9076, .F. ) ;
#2081 = ORIENTED_EDGE ( 'NONE', *, *, #10640, .T. ) ;
#2082 = CARTESIAN_POINT ( 'NONE',  ( 0.000000000000000000, 4.177097350749890303, -6.108343287861167425 ) ) ;
#2083 = DIRECTION ( 'NONE',  ( -1.000000000000000000, 1.010728034814421376E-30, 1.090846720500930387E-30 ) ) ;
#2084 = CARTESIAN_POINT ( 'NONE',  ( 20.00000000000006750, -2.500000000000000000, -20.00000000000000000 ) ) ;
#2085 = DIRECTION ( 'NONE',  ( -1.000000000000000000, 1.010728034814421376E-30, 1.090846720500930387E-30 ) ) ;
#2086 = ORIENTED_EDGE ( 'NONE', *, *, #10039, .T. ) ;
#2087 = DIRECTION ( 'NONE',  ( -2.465190328815656418E-32, 1.177425296209236734E-30, 1.000000000000000000 ) ) ;
#2088 = AXIS2_PLACEMENT_3D ( 'NONE', #1286, #5281, #131 ) ;
#2089 = DIRECTION ( 'NONE',  ( 0.000000000000000000, 0.000000000000000000, -1.000000000000000000 ) ) ;
#2090 = CIRCLE ( 'NONE', #5171, 6.499000000000009436 ) ;
#2091 = CARTESIAN_POINT ( 'NONE',  ( -10.00000000000000178, 0.000000000000000000, 0.000000000000000000 ) ) ;
#2092 = VERTEX_POINT ( 'NONE', #9392 ) ;
#2093 = EDGE_CURVE ( 'NONE', #6823, #9939, #4104, .T. ) ;
#2094 = ORIENTED_EDGE ( 'NONE', *, *, #368, .F. ) ;
#2095 = DIRECTION ( 'NONE',  ( -1.000000000000000000, 1.010728034814421376E-30, 1.090846720500930387E-30 ) ) ;
#2096 = VERTEX_POINT ( 'NONE', #12516 ) ;
#2097 = ORIENTED_EDGE ( 'NONE', *, *, #5025, .T. ) ;
#2098 = APPLICATION_PROTOCOL_DEFINITION ( 'draft international standard', 'automotive_design', 1998, #2825 ) ;
#2099 = CYLINDRICAL_SURFACE ( 'NONE', #4316, 7.400000000000010125 ) ;
#2100 = ORIENTED_EDGE ( 'NONE', *, *, #8298, .F. ) ;
#2101 = DIRECTION ( 'NONE',  ( -1.000000000000000000, -1.031065855027150586E-29, 2.218671295934095703E-30 ) ) ;
#2102 = ADVANCED_FACE ( 'NONE', ( #7546 ), #1685, .T. ) ;
#2103 = LINE ( 'NONE', #4160, #8896 ) ;
#2104 = AXIS2_PLACEMENT_3D ( 'NONE', #10365, #4392, #10559 ) ;
#2105 = VERTEX_POINT ( 'NONE', #716 ) ;
#2106 = PLANE ( 'NONE',  #5291 ) ;
#2107 = DIRECTION ( 'NONE',  ( -1.000000000000000000, 1.010728034814421376E-30, 1.090846720500930387E-30 ) ) ;
#2108 = ORIENTED_EDGE ( 'NONE', *, *, #12483, .T. ) ;
#2109 = CLOSED_SHELL ( 'NONE', ( #3239, #7662, #9087, #11025, #1267, #7819 ) ) ;
#2110 = EDGE_CURVE ( 'NONE', #229, #3731, #11310, .T. ) ;
#2111 = ORIENTED_EDGE ( 'NONE', *, *, #4710, .T. ) ;
#2112 = ORIENTED_EDGE ( 'NONE', *, *, #6635, .F. ) ;
#2113 = CIRCLE ( 'NONE', #52, 2.800000000000003819 ) ;
#2114 = ADVANCED_FACE ( 'NONE', ( #11552 ), #3566, .T. ) ;
#2115 = ORIENTED_EDGE ( 'NONE', *, *, #3812, .F. ) ;
#2116 = ADVANCED_FACE ( 'NONE', ( #9461 ), #3629, .T. ) ;
#2117 = CARTESIAN_POINT ( 'NONE',  ( -30.00000000000000000, 0.000000000000000000, 2.185182530847200403E-15 ) ) ;
#2118 = CARTESIAN_POINT ( 'NONE',  ( -4.235886605889374046, -2.417314728048561179, -3.751161874094032456 ) ) ;
#2119 = VERTEX_POINT ( 'NONE', #8576 ) ;
#2120 = EDGE_CURVE ( 'NONE', #3178, #1849, #7206, .T. ) ;
#2121 = DIRECTION ( 'NONE',  ( 0.000000000000000000, 0.000000000000000000, -1.000000000000000000 ) ) ;
#2122 = ORIENTED_EDGE ( 'NONE', *, *, #3535, .T. ) ;
#2123 = DIRECTION ( 'NONE',  ( -1.000000000000000000, 1.010728034814421376E-30, 1.090846720500930387E-30 ) ) ;
#2124 = AXIS2_PLACEMENT_3D ( 'NONE', #11803, #5926, #1875 ) ;
#2125 = CARTESIAN_POINT ( 'NONE',  ( 19.99999999999999645, -4.518585619147844845, -5.860237538055132589 ) ) ;
#2126 = CARTESIAN_POINT ( 'NONE',  ( 19.99999999999999645, 0.000000000000000000, 0.000000000000000000 ) ) ;
#2127 = VERTEX_POINT ( 'NONE', #6657 ) ;
#2128 = CARTESIAN_POINT ( 'NONE',  ( 33.00000000000001421, 39.34792583643766761, -19.56347054209567204 ) ) ;
#2129 = AXIS2_PLACEMENT_3D ( 'NONE', #3401, #12344, #3645 ) ;
#2130 = VERTEX_POINT ( 'NONE', #777 ) ;
#2131 = DIRECTION ( 'NONE',  ( 0.000000000000000000, -1.530455820933490821E-32, 1.000000000000000000 ) ) ;
#2132 =( LENGTH_UNIT ( ) NAMED_UNIT ( * ) SI_UNIT ( .MILLI., .METRE. ) );
#2133 = FACE_BOUND ( 'NONE', #2564, .T. ) ;
#2134 = CARTESIAN_POINT ( 'NONE',  ( 4.000000000000000000, 0.000000000000000000, 0.000000000000000000 ) ) ;
#2135 = CIRCLE ( 'NONE', #9516, 2.800000000000002931 ) ;
#2136 = FACE_OUTER_BOUND ( 'NONE', #5986, .T. ) ;
#2137 = CARTESIAN_POINT ( 'NONE',  ( 6.000000000000000000, 49.63999999999998636, -5.000000000000000888 ) ) ;
#2138 = CARTESIAN_POINT ( 'NONE',  ( 11.00000000000003375, -19.99999999999999645, 14.15000000000003411 ) ) ;
#2139 = LINE ( 'NONE', #3943, #3312 ) ;
#2140 = AXIS2_PLACEMENT_3D ( 'NONE', #10176, #7310, #7248 ) ;
#2141 = CARTESIAN_POINT ( 'NONE',  ( 0.000000000000000000, 2.796709610837340598, 6.851161606081848987 ) ) ;
#2142 = CIRCLE ( 'NONE', #10562, 7.400000000000009237 ) ;
#2143 =( NAMED_UNIT ( * ) PLANE_ANGLE_UNIT ( ) SI_UNIT ( $, .RADIAN. ) );
#2144 = APPLICATION_CONTEXT ( 'automotive_design' ) ;
#2145 = ORIENTED_EDGE ( 'NONE', *, *, #10412, .T. ) ;
#2146 = FACE_OUTER_BOUND ( 'NONE', #7765, .T. ) ;
#2147 = EDGE_CURVE ( 'NONE', #12369, #1954, #4712, .T. ) ;
#2148 = DIRECTION ( 'NONE',  ( -1.000000000000000000, -2.206481006425900381E-16, 8.674603474570137221E-17 ) ) ;
#2150 = DIRECTION ( 'NONE',  ( -1.000000000000000000, 1.006188713385347367E-17, 3.844790828812615713E-17 ) ) ;
#2149 = AXIS2_PLACEMENT_3D ( 'NONE', #5413, #5544, #12384 ) ;
#2151 = CARTESIAN_POINT ( 'NONE',  ( 0.000000000000000000, -1.268072931708545736, 6.374087545670214183 ) ) ;
#2152 = DIRECTION ( 'NONE',  ( 0.000000000000000000, -1.530455820933490821E-32, 1.000000000000000000 ) ) ;
#2153 = EDGE_LOOP ( 'NONE', ( #101, #3167 ) ) ;
#2154 = CIRCLE ( 'NONE', #8323, 2.800000000000003819 ) ;
#2155 = DIRECTION ( 'NONE',  ( 0.000000000000000000, 0.000000000000000000, -1.000000000000000000 ) ) ;
#2156 = CARTESIAN_POINT ( 'NONE',  ( 11.00000000000003375, -19.99999999999999645, 12.00000000000003553 ) ) ;
#2157 = LINE ( 'NONE', #3013, #9658 ) ;
#2158 = ORIENTED_EDGE ( 'NONE', *, *, #3957, .T. ) ;
#2159 = DIRECTION ( 'NONE',  ( -1.000000000000000000, 1.010728034814421376E-30, 1.090846720500930387E-30 ) ) ;
#2160 = VERTEX_POINT ( 'NONE', #5421 ) ;
#2161 = AXIS2_PLACEMENT_3D ( 'NONE', #8036, #7219, #7085 ) ;
#2162 = VERTEX_POINT ( 'NONE', #12325 ) ;
#2163 = APPLICATION_PROTOCOL_DEFINITION ( 'draft international standard', 'automotive_design', 1998, #4366 ) ;
#2164 = AXIS2_PLACEMENT_3D ( 'NONE', #10726, #8862, #5970 ) ;
#2165 = CARTESIAN_POINT ( 'NONE',  ( 40.00000000000000711, 22.56100271565320980, -6.249672610153679919 ) ) ;
#2166 = ORIENTED_EDGE ( 'NONE', *, *, #7676, .T. ) ;
#2167 = CARTESIAN_POINT ( 'NONE',  ( -45.00000000000013500, 30.00000000000000000, 3.443468848353505426E-15 ) ) ;
#2168 = CARTESIAN_POINT ( 'NONE',  ( 19.99999999999997868, 0.2252065540230664964, -6.573992004634869879 ) ) ;
#2169 = EDGE_CURVE ( 'NONE', #2162, #10498, #1654, .T. ) ;
#2170 = VERTEX_POINT ( 'NONE', #841 ) ;
#2171 = DIRECTION ( 'NONE',  ( -1.848892746611746419E-31, -1.000000000000000000, 3.250006781153460502E-32 ) ) ;
#2173 = CARTESIAN_POINT ( 'NONE',  ( 9.999999999999994671, -1.113123845672416401, 7.315801754025030412 ) ) ;
#2172 = PRODUCT_RELATED_PRODUCT_CATEGORY ( 'part', '', ( #11216 ) ) ;
#2174 = DIRECTION ( 'NONE',  ( -0.000000000000000000, -0.000000000000000000, -1.000000000000000000 ) ) ;
#2175 = CARTESIAN_POINT ( 'NONE',  ( 19.99999999999999645, -6.486618105788070743, -0.4009819817180210189 ) ) ;
#2176 = CIRCLE ( 'NONE', #4432, 6.499000000000008548 ) ;
#2177 = ORIENTED_EDGE ( 'NONE', *, *, #8399, .F. ) ;
#2178 = ORIENTED_EDGE ( 'NONE', *, *, #5293, .T. ) ;
#2179 = ORIENTED_EDGE ( 'NONE', *, *, #10492, .F. ) ;
#2180 = ORIENTED_EDGE ( 'NONE', *, *, #9546, .F. ) ;
#2181 = CARTESIAN_POINT ( 'NONE',  ( 27.00000000000000355, 39.34792583643766051, -17.06347054209567915 ) ) ;
#2182 = CARTESIAN_POINT ( 'NONE',  ( -0.5636800770139697159, -4.293361309318505903, -3.531542292955881734 ) ) ;
#2183 = EDGE_LOOP ( 'NONE', ( #11415, #8143, #11917, #10065 ) ) ;
#2184 = EDGE_CURVE ( 'NONE', #9120, #8530, #2066, .T. ) ;
#2185 = DIRECTION ( 'NONE',  ( 0.000000000000000000, -1.000000000000000000, -1.530455820933490821E-32 ) ) ;
#2186 = ORIENTED_EDGE ( 'NONE', *, *, #9830, .T. ) ;
#2187 = EDGE_CURVE ( 'NONE', #3764, #6793, #6906, .T. ) ;
#2188 = FACE_OUTER_BOUND ( 'NONE', #12740, .T. ) ;
#2189 = EDGE_CURVE ( 'NONE', #11297, #3706, #10268, .T. ) ;
#2190 = FACE_OUTER_BOUND ( 'NONE', #11323, .T. ) ;
#2191 = VECTOR ( 'NONE', #2556, 1000.000000000000000 ) ;
#2192 = DIRECTION ( 'NONE',  ( -1.000000000000000000, 1.010728034814421376E-30, 1.090846720500930387E-30 ) ) ;
#2193 = ADVANCED_FACE ( 'NONE', ( #3115 ), #11861, .T. ) ;
#2194 = PRESENTATION_LAYER_ASSIGNMENT (  '', '', ( #1772 ) ) ;
#2195 = ORIENTED_EDGE ( 'NONE', *, *, #10516, .F. ) ;
#2196 = FACE_OUTER_BOUND ( 'NONE', #11712, .T. ) ;
#2197 = ORIENTED_EDGE ( 'NONE', *, *, #414, .F. ) ;
#2198 = CARTESIAN_POINT ( 'NONE',  ( 33.00000000000001421, 81.84122341717352356, -27.68198508464163510 ) ) ;
#2199 =( NAMED_UNIT ( * ) SI_UNIT ( $, .STERADIAN. ) SOLID_ANGLE_UNIT ( ) );
#2200 = DIRECTION ( 'NONE',  ( -0.8660254037844373753, 0.5000000000000021094, 0.000000000000000000 ) ) ;
#2201 = AXIS2_PLACEMENT_3D ( 'NONE', #7197, #11119, #2305 ) ;
#2202 = EDGE_CURVE ( 'NONE', #2374, #7064, #6800, .T. ) ;
#2203 = CARTESIAN_POINT ( 'NONE',  ( 19.99999999999999645, 0.000000000000000000, 0.000000000000000000 ) ) ;
#2204 = VECTOR ( 'NONE', #1108, 1000.000000000000000 ) ;
#2205 = EDGE_CURVE ( 'NONE', #4950, #5083, #2930, .T. ) ;
#2206 = ADVANCED_BREP_SHAPE_REPRESENTATION ( '', ( #5705, #12422 ), #2062 ) ;
#2207 = CARTESIAN_POINT ( 'NONE',  ( -17.00000000000002842, 19.99999999999998579, 12.00000000000003730 ) ) ;
#2208 = CARTESIAN_POINT ( 'NONE',  ( 0.000000000000000000, 2.796709610837448068, -6.851161606081825006 ) ) ;
#2209 = CARTESIAN_POINT ( 'NONE',  ( 32.99999999999999289, 39.34792583643766051, -19.21347054209566707 ) ) ;
#2210 = PRODUCT_DEFINITION_FORMATION_WITH_SPECIFIED_SOURCE ( 'ANY', '', #4538, .NOT_KNOWN. ) ;
#2211 = DIRECTION ( 'NONE',  ( -0.000000000000000000, -1.530455820933490821E-32, 1.000000000000000000 ) ) ;
#2212 = VECTOR ( 'NONE', #3263, 1000.000000000000000 ) ;
#2213 = CARTESIAN_POINT ( 'NONE',  ( 6.000000000000000000, 49.63999999999998636, -13.00000000000000178 ) ) ;
#2214 = ORIENTED_EDGE ( 'NONE', *, *, #6084, .F. ) ;
#2215 = DIRECTION ( 'NONE',  ( -1.000000000000000000, 1.010728034814421376E-30, 1.090846720500930387E-30 ) ) ;
#2216 = DIRECTION ( 'NONE',  ( -8.073498326871283938E-31, -0.2660368455666825005, 0.9639628606958513535 ) ) ;
#2217 = DIRECTION ( 'NONE',  ( -1.000000000000000000, 1.010728034814421376E-30, 1.090846720500930387E-30 ) ) ;
#2218 = DIRECTION ( 'NONE',  ( 0.000000000000000000, 0.9989930665413144784, 0.04486483035051876817 ) ) ;
#2219 = ORIENTED_EDGE ( 'NONE', *, *, #9775, .F. ) ;
#2220 = CONICAL_SURFACE ( 'NONE', #8179, 2.500000000000000888, 0.9599310885968785900 ) ;
#2221 = ADVANCED_FACE ( 'NONE', ( #8948 ), #10813, .T. ) ;
#2222 = CARTESIAN_POINT ( 'NONE',  ( -18.00000000000002842, 30.00000000000000000, 2.000000000000004441 ) ) ;
#2223 = FACE_OUTER_BOUND ( 'NONE', #5328, .T. ) ;
#2224 = EDGE_CURVE ( 'NONE', #6542, #8459, #3712, .T. ) ;
#2225 = DIRECTION ( 'NONE',  ( 0.000000000000000000, -1.000000000000000000, 0.000000000000000000 ) ) ;
#2226 = ORIENTED_EDGE ( 'NONE', *, *, #7584, .T. ) ;
#2227 = DIRECTION ( 'NONE',  ( -1.000000000000000000, 1.010728034814421376E-30, 1.090846720500930387E-30 ) ) ;
#2228 = VERTEX_POINT ( 'NONE', #8764 ) ;
#2229 = ORIENTED_EDGE ( 'NONE', *, *, #4099, .F. ) ;
#2230 = ITEM_DEFINED_TRANSFORMATION ( 'NONE', 'NONE', #7349,  #12422 ) ;
#2231 = CARTESIAN_POINT ( 'NONE',  ( 28.99999999999999645, 3.469446951953614189E-15, 0.000000000000000000 ) ) ;
#2232 = EDGE_LOOP ( 'NONE', ( #3487, #155, #2650, #1915 ) ) ;
#2233 = DIRECTION ( 'NONE',  ( -1.000000000000000000, -5.916456789157575403E-31, 1.577021341797099039E-16 ) ) ;
#2234 = ORIENTED_EDGE ( 'NONE', *, *, #7074, .F. ) ;
#2235 = CARTESIAN_POINT ( 'NONE',  ( 19.99999999999997868, -3.178467454237100309, -5.758943784352606343 ) ) ;
#2236 = LINE ( 'NONE', #231, #4108 ) ;
#2237 = CARTESIAN_POINT ( 'NONE',  ( 0.000000000000000000, 6.424561140605085541, 0.9808237102696959475 ) ) ;
#2238 = CARTESIAN_POINT ( 'NONE',  ( 4.204015924366190760, -1.626724848190935324, -3.610627190413396193 ) ) ;
#2239 = ORIENTED_EDGE ( 'NONE', *, *, #11747, .F. ) ;
#2240 = ORIENTED_EDGE ( 'NONE', *, *, #1641, .F. ) ;
#2241 = EDGE_CURVE ( 'NONE', #4528, #5879, #11115, .T. ) ;
#2242 = VERTEX_POINT ( 'NONE', #11801 ) ;
#2243 = ADVANCED_FACE ( 'NONE', ( #7029 ), #5797, .T. ) ;
#2244 = EDGE_CURVE ( 'NONE', #11848, #1577, #6964, .T. ) ;
#2245 = VERTEX_POINT ( 'NONE', #4902 ) ;
#2246 = CARTESIAN_POINT ( 'NONE',  ( 40.00000000000000711, 14.86906044972263707, -7.469374795321336080 ) ) ;
#2247 = EDGE_CURVE ( 'NONE', #2437, #7453, #7218, .T. ) ;
#2248 = VECTOR ( 'NONE', #1900, 1000.000000000000000 ) ;
#2249 = DIRECTION ( 'NONE',  ( 0.000000000000000000, 0.000000000000000000, -1.000000000000000000 ) ) ;
#2250 = ORIENTED_EDGE ( 'NONE', *, *, #666, .F. ) ;
#2251 = DIRECTION ( 'NONE',  ( 0.000000000000000000, 0.000000000000000000, 1.000000000000000000 ) ) ;
#2252 = ORIENTED_EDGE ( 'NONE', *, *, #8762, .T. ) ;
#2253 = CARTESIAN_POINT ( 'NONE',  ( 1.734723475976807094E-14, -3.469446951953614189E-15, -4.000000000000010658 ) ) ;
#2254 = CARTESIAN_POINT ( 'NONE',  ( 4.141042297810618500, -2.227970268150431643, -3.687027686973626928 ) ) ;
#2255 = VECTOR ( 'NONE', #5483, 999.9999999999998863 ) ;
#2256 = AXIS2_PLACEMENT_3D ( 'NONE', #3479, #11264, #10340 ) ;
#2257 = VECTOR ( 'NONE', #11038, 1000.000000000000000 ) ;
#2258 = DIRECTION ( 'NONE',  ( 1.000000000000000000, 0.000000000000000000, 0.000000000000000000 ) ) ;
#2259 = EDGE_LOOP ( 'NONE', ( #7198, #5294, #108, #7736 ) ) ;
#2260 = CARTESIAN_POINT ( 'NONE',  ( 3.054370817402599269E-30, -6.577476285968334224, 2.730038749994992742 ) ) ;
#2261 = EDGE_CURVE ( 'NONE', #11340, #4626, #5032, .T. ) ;
#2262 = ORIENTED_EDGE ( 'NONE', *, *, #1795, .T. ) ;
#2263 = DIRECTION ( 'NONE',  ( -1.000000000000000000, 1.010728034814421376E-30, 1.090846720500930387E-30 ) ) ;
#2264 = SURFACE_STYLE_FILL_AREA ( #2456 ) ;
#2265 = PLANE ( 'NONE',  #4114 ) ;
#2266 = AXIS2_PLACEMENT_3D ( 'NONE', #2126, #6048, #9959 ) ;
#2267 = CIRCLE ( 'NONE', #2053, 2.800000000000003819 ) ;
#2268 = AXIS2_PLACEMENT_3D ( 'NONE', #2737, #9587, #2538 ) ;
#2269 = CARTESIAN_POINT ( 'NONE',  ( 40.00000000000000000, 39.34792583643766051, -17.06347054209567915 ) ) ;
#2270 = EDGE_CURVE ( 'NONE', #12673, #9454, #12708, .T. ) ;
#2271 = CARTESIAN_POINT ( 'NONE',  ( -1.999999999999990008, -3.464101615137811230, -3.142992957459264325 ) ) ;
#2272 = FACE_OUTER_BOUND ( 'NONE', #4673, .T. ) ;
#2273 = FACE_OUTER_BOUND ( 'NONE', #1529, .T. ) ;
#2274 = DIRECTION ( 'NONE',  ( -1.000000000000000000, 1.010728034814421376E-30, 1.090846720500930387E-30 ) ) ;
#2275 = PRESENTATION_LAYER_ASSIGNMENT (  '', '', ( #12153 ) ) ;
#2276 = AXIS2_PLACEMENT_3D ( 'NONE', #5092, #4833, #11795 ) ;
#2277 = AXIS2_PLACEMENT_3D ( 'NONE', #9966, #11016, #8044 ) ;
#2278 = EDGE_CURVE ( 'NONE', #6542, #6552, #7978, .T. ) ;
#2279 = CARTESIAN_POINT ( 'NONE',  ( 12.94787914004602847, -12.49999999999999645, 5.638155724715463890 ) ) ;
#2280 = EDGE_CURVE ( 'NONE', #11065, #6291, #12156, .T. ) ;
#2281 = ORIENTED_EDGE ( 'NONE', *, *, #2261, .T. ) ;
#2282 = CARTESIAN_POINT ( 'NONE',  ( 4.200000000000001954, 0.000000000000000000, -1.734723475976807094E-14 ) ) ;
#2283 = LINE ( 'NONE', #11880, #2343 ) ;
#2284 = COLOUR_RGB ( '', 0.72549020, 0.75294118, 0.79215686) ;
#2285 = MECHANICAL_DESIGN_GEOMETRIC_PRESENTATION_REPRESENTATION (  '', ( #5766 ), #6810 ) ;
#2286 = CARTESIAN_POINT ( 'NONE',  ( -3.999999999999992895, 1.677772373332863332, -3.535253723896553790 ) ) ;
#2287 = DIRECTION ( 'NONE',  ( -1.000000000000000000, 0.000000000000000000, 0.000000000000000000 ) ) ;
#2288 = ORIENTED_EDGE ( 'NONE', *, *, #11408, .F. ) ;
#2289 = DIRECTION ( 'NONE',  ( -1.000000000000000000, -1.081682119347366197E-16, 6.938893903907228378E-17 ) ) ;
#2290 = FACE_OUTER_BOUND ( 'NONE', #9866, .T. ) ;
#2291 = CARTESIAN_POINT ( 'NONE',  ( 2.000000000000001776, -1.329782007511007169, -0.7677499999999976010 ) ) ;
#2292 = ORIENTED_EDGE ( 'NONE', *, *, #2811, .F. ) ;
#2293 = DIRECTION ( 'NONE',  ( -1.000000000000000000, 1.010728034814421376E-30, 1.090846720500930387E-30 ) ) ;
#2294 = ORIENTED_EDGE ( 'NONE', *, *, #6065, .F. ) ;
#2295 = COLOUR_RGB ( '', 0.40784314, 0.44705882, 0.49803922) ;
#2296 = ORIENTED_EDGE ( 'NONE', *, *, #10876, .F. ) ;
#2297 = ITEM_DEFINED_TRANSFORMATION ( 'NONE', 'NONE', #6110,  #12422 ) ;
#2298 = DIRECTION ( 'NONE',  ( -1.000000000000000000, 1.010728034814421376E-30, 1.090846720500930387E-30 ) ) ;
#2299 = ORIENTED_EDGE ( 'NONE', *, *, #5405, .F. ) ;
#2300 = DIRECTION ( 'NONE',  ( 0.000000000000000000, 0.000000000000000000, -1.000000000000000000 ) ) ;
#2301 = EDGE_CURVE ( 'NONE', #10144, #7729, #4839, .T. ) ;
#2302 = DIRECTION ( 'NONE',  ( 0.000000000000000000, 0.000000000000000000, 1.000000000000000000 ) ) ;
#2303 = DIRECTION ( 'NONE',  ( 0.000000000000000000, 0.000000000000000000, -1.000000000000000000 ) ) ;
#2304 = CARTESIAN_POINT ( 'NONE',  ( -31.74999999999995026, 0.000000000000000000, 6.938893903907228378E-15 ) ) ;
#2305 = DIRECTION ( 'NONE',  ( 0.000000000000000000, 0.000000000000000000, 1.000000000000000000 ) ) ;
#2306 = CARTESIAN_POINT ( 'NONE',  ( 2.000000000000001776, 1.773042676681341856, -3.469446951953614189E-15 ) ) ;
#2307 = AXIS2_PLACEMENT_3D ( 'NONE', #8456, #9535, #3641 ) ;
#2308 = ORIENTED_EDGE ( 'NONE', *, *, #9718, .F. ) ;
#2309 = EDGE_LOOP ( 'NONE', ( #1929, #8849, #11954, #2723 ) ) ;
#2310 = ORIENTED_EDGE ( 'NONE', *, *, #5875, .T. ) ;
#2311 = ORIENTED_EDGE ( 'NONE', *, *, #8517, .F. ) ;
#2312 = AXIS2_PLACEMENT_3D ( 'NONE', #3373, #579, #7475 ) ;
#2313 = CARTESIAN_POINT ( 'NONE',  ( 2.000000000000091926, 0.8865213383406691516, -1.535500000000002085 ) ) ;
#2314 = CIRCLE ( 'NONE', #11775, 2.800000000000002931 ) ;
#2315 = CARTESIAN_POINT ( 'NONE',  ( 15.00000000000003375, 30.00000000000001776, -9.742497179615118866E-31 ) ) ;
#2316 = ORIENTED_EDGE ( 'NONE', *, *, #7837, .T. ) ;
#2317 = CYLINDRICAL_SURFACE ( 'NONE', #6387, 7.400000000000010125 ) ;
#2318 = ORIENTED_EDGE ( 'NONE', *, *, #4711, .T. ) ;
#2319 = CARTESIAN_POINT ( 'NONE',  ( -3.355112389629172576, 2.681727112203154739, -0.2256878752776703412 ) ) ;
#2320 = ADVANCED_FACE ( 'NONE', ( #7797 ), #9776, .T. ) ;
#2321 = CARTESIAN_POINT ( 'NONE',  ( 11.00000000000003375, -6.123233995736745575E-16, 20.00000000000003553 ) ) ;
#2322 = ADVANCED_FACE ( 'NONE', ( #6055 ), #5221, .T. ) ;
#2323 = FACE_OUTER_BOUND ( 'NONE', #2841, .T. ) ;
#2324 = AXIS2_PLACEMENT_3D ( 'NONE', #9320, #4378, #10287 ) ;
#2325 = DIRECTION ( 'NONE',  ( -1.000000000000000000, 1.010728034814421376E-30, 1.090846720500930387E-30 ) ) ;
#2326 = ORIENTED_EDGE ( 'NONE', *, *, #877, .T. ) ;
#2327 = CARTESIAN_POINT ( 'NONE',  ( 19.99999999999999645, 1.052479792859053020, 6.413211932068313637 ) ) ;
#2328 = VERTEX_POINT ( 'NONE', #11991 ) ;
#2329 = DIRECTION ( 'NONE',  ( -3.437775699846489820E-17, -0.2951046417778627751, -0.9554649393887560960 ) ) ;
#2330 = CIRCLE ( 'NONE', #2535, 3.299999999999999822 ) ;
#2331 = DIRECTION ( 'NONE',  ( -1.000000000000000000, 1.010728034814421376E-30, 1.090846720500930387E-30 ) ) ;
#2332 = AXIS2_PLACEMENT_3D ( 'NONE', #1670, #638, #4577 ) ;
#2333 = CARTESIAN_POINT ( 'NONE',  ( 14.00000000000000000, 30.00000000000000000, 0.000000000000000000 ) ) ;
#2334 = EDGE_CURVE ( 'NONE', #271, #7997, #9244, .T. ) ;
#2335 = DIRECTION ( 'NONE',  ( -1.000000000000000000, 1.010728034814421376E-30, 1.090846720500930387E-30 ) ) ;
#2336 = FACE_OUTER_BOUND ( 'NONE', #3673, .T. ) ;
#2337 = AXIS2_PLACEMENT_3D ( 'NONE', #8338, #6411, #8274 ) ;
#2338 = DIRECTION ( 'NONE',  ( 1.000000000000000000, 1.081682119347366321E-16, -5.551115123125780237E-17 ) ) ;
#2339 = ORIENTED_EDGE ( 'NONE', *, *, #11234, .F. ) ;
#2340 = DIRECTION ( 'NONE',  ( 0.000000000000000000, 0.000000000000000000, 1.000000000000000000 ) ) ;
#2341 = DIRECTION ( 'NONE',  ( 0.3420201433256680468, 7.946868433027814422E-32, -0.9396926207859086499 ) ) ;
#2342 =( NAMED_UNIT ( * ) SI_UNIT ( $, .STERADIAN. ) SOLID_ANGLE_UNIT ( ) );
#2343 = VECTOR ( 'NONE', #1237, 999.9999999999998863 ) ;
#2344 = EDGE_LOOP ( 'NONE', ( #12568, #3684 ) ) ;
#2345 = EDGE_CURVE ( 'NONE', #927, #8673, #9017, .T. ) ;
#2346 = CARTESIAN_POINT ( 'NONE',  ( 27.00000000000001421, 81.84122341717352356, -27.68198508464163510 ) ) ;
#2347 = CYLINDRICAL_SURFACE ( 'NONE', #11394, 2.800000000000003819 ) ;
#2348 = DIRECTION ( 'NONE',  ( 0.000000000000000000, -0.9749279121818260618, 0.2225209339563040956 ) ) ;
#2349 = EDGE_CURVE ( 'NONE', #5519, #9099, #1435, .T. ) ;
#2350 = LINE ( 'NONE', #592, #5900 ) ;
#2351 = DIRECTION ( 'NONE',  ( 0.000000000000000000, 0.000000000000000000, 1.000000000000000000 ) ) ;
#2352 = EDGE_CURVE ( 'NONE', #1661, #235, #12058, .T. ) ;
#2353 = LINE ( 'NONE', #10308, #1524 ) ;
#2354 = ADVANCED_FACE ( 'NONE', ( #324, #10031, #2133, #8247 ), #8180, .T. ) ;
#2355 = SURFACE_STYLE_USAGE ( .BOTH. , #11170 ) ;
#2356 = CIRCLE ( 'NONE', #12436, 2.800000000000002931 ) ;
#2357 = B_SPLINE_CURVE_WITH_KNOTS ( 'NONE', 3,
 ( #4059, #12178, #11930, #10146, #2386, #8951, #10344, #1338 ),
 .UNSPECIFIED., .F., .F.,
 ( 4, 2, 2, 4 ),
 ( 0.000000000000000000, 0.002450665683189820563, 0.003675998524784731061, 0.004901331366379641993 ),
 .UNSPECIFIED. ) ;
#2358 = ORIENTED_EDGE ( 'NONE', *, *, #7362, .T. ) ;
#2359 = EDGE_CURVE ( 'NONE', #1763, #10769, #4190, .T. ) ;
#2360 = CARTESIAN_POINT ( 'NONE',  ( 33.00000000000001421, 70.57443853988016258, -5.364737079370081041 ) ) ;
#2361 = ORIENTED_EDGE ( 'NONE', *, *, #4033, .T. ) ;
#2362 = EDGE_LOOP ( 'NONE', ( #3841, #7184, #3552, #6393 ) ) ;
#2363 = ITEM_DEFINED_TRANSFORMATION ( 'NONE', 'NONE', #11871,  #12422 ) ;
#2364 = EDGE_LOOP ( 'NONE', ( #7780, #6932, #6499, #12596, #9572, #5402, #6108, #11207, #11988, #1264, #5955, #8102, #319, #12564, #7240, #3207, #9224, #3930, #7017, #10431, #51, #9507, #6444, #9945, #4832, #3721, #11830, #4410, #11404, #351, #5306, #4986, #7843, #2435, #7250, #1920, #5689, #2968, #5450, #5849, #2424, #1963, #12260, #4749, #9685, #8609, #9549, #6926, #5783, #683, #10681, #11238, #10058, #5820, #4546, #5242, #2443, #5579, #1379, #5590, #8026, #9021, #8697, #8412, #10539, #11469, #7440, #6180, #2294, #1909, #1009, #12531, #2823, #6226, #651, #10123, #6033, #9088, #1481, #12405, #12579, #9124, #7324, #9177, #6150, #6744, #236, #9299, #1491, #11263, #7519, #11520, #9952, #285, #2115, #7654, #3486, #1833, #1697, #869, #3457, #10205, #10332, #429, #5669, #3475, #5921, #9854, #11787, #5984, #2685, #9446, #6712, #8983, #1774, #6178, #10264, #7690, #5385, #2229, #6540, #10859, #7890, #8521, #6042, #10939, #6334, #4943, #6868, #6806, #1311, #11511, #4037, #5608, #5178, #9474, #5386, #1857, #3581, #857, #5915, #9947, #11140, #5287 ) ) ;
#2365 = AXIS2_PLACEMENT_3D ( 'NONE', #2156, #6804, #3958 ) ;
#2366 =( LENGTH_UNIT ( ) NAMED_UNIT ( * ) SI_UNIT ( .MILLI., .METRE. ) );
#2367 = LINE ( 'NONE', #4480, #10342 ) ;
#2368 = FACE_OUTER_BOUND ( 'NONE', #10655, .T. ) ;
#2369 = CARTESIAN_POINT ( 'NONE',  ( 20.00000000000000000, 10.63631887905125950, -9.927230231572497843 ) ) ;
#2370 = FACE_OUTER_BOUND ( 'NONE', #9107, .T. ) ;
#2371 = VERTEX_POINT ( 'NONE', #11078 ) ;
#2372 = CARTESIAN_POINT ( 'NONE',  ( -4.175648173966062693, 2.207990556236520518, -3.469390959564077725 ) ) ;
#2373 = PLANE ( 'NONE',  #10491 ) ;
#2374 = VERTEX_POINT ( 'NONE', #257 ) ;
#2375 = CIRCLE ( 'NONE', #8106, 4.000000000000000000 ) ;
#2376 = AXIS2_PLACEMENT_3D ( 'NONE', #7461, #10409, #1596 ) ;
#2377 = ORIENTED_EDGE ( 'NONE', *, *, #687, .T. ) ;
#2378 = VERTEX_POINT ( 'NONE', #4125 ) ;
#2379 = ORIENTED_EDGE ( 'NONE', *, *, #6174, .T. ) ;
#2380 = LINE ( 'NONE', #4172, #2959 ) ;
#2381 = ORIENTED_EDGE ( 'NONE', *, *, #2850, .T. ) ;
#2382 = DIRECTION ( 'NONE',  ( 0.000000000000000000, 0.000000000000000000, 1.000000000000000000 ) ) ;
#2383 = ORIENTED_EDGE ( 'NONE', *, *, #382, .T. ) ;
#2384 = AXIS2_PLACEMENT_3D ( 'NONE', #12179, #9066, #11136 ) ;
#2385 = CARTESIAN_POINT ( 'NONE',  ( -4.000000000000001776, 2.309401076758498039, -0.4999999999999935052 ) ) ;
#2386 = CARTESIAN_POINT ( 'NONE',  ( -1.393927851585486266, 4.043713361053526079, -3.526374918436849359 ) ) ;
#2387 = ADVANCED_FACE ( 'NONE', ( #4252 ), #2265, .F. ) ;
#2388 = CARTESIAN_POINT ( 'NONE',  ( 0.000000000000000000, 4.192831774279053292, -4.965597920955355349 ) ) ;
#2389 = FACE_OUTER_BOUND ( 'NONE', #5721, .T. ) ;
#2390 = EDGE_LOOP ( 'NONE', ( #9885, #4090, #6511, #7356 ) ) ;
#2391 = ORIENTED_EDGE ( 'NONE', *, *, #2184, .T. ) ;
#2392 = AXIS2_PLACEMENT_3D ( 'NONE', #6722, #12712, #5872 ) ;
#2393 = DIRECTION ( 'NONE',  ( 0.000000000000000000, 0.000000000000000000, -1.000000000000000000 ) ) ;
#2394 = DIRECTION ( 'NONE',  ( 0.000000000000000000, -0.1785568947986228838, -0.9839295885986322210 ) ) ;
#2395 = DIRECTION ( 'NONE',  ( -1.000000000000000000, 0.000000000000000000, 1.224646799147352714E-16 ) ) ;
#2396 = CARTESIAN_POINT ( 'NONE',  ( 19.99999999999999645, -3.612733913993637636, 6.458185013351672055 ) ) ;
#2397 = APPLICATION_CONTEXT ( 'automotive_design' ) ;
#2398 = DIRECTION ( 'NONE',  ( -1.000000000000000000, 1.010728034814421376E-30, 1.090846720500930387E-30 ) ) ;
#2399 = PLANE ( 'NONE',  #4713 ) ;
#2400 = ORIENTED_EDGE ( 'NONE', *, *, #8367, .F. ) ;
#2401 = FACE_OUTER_BOUND ( 'NONE', #9363, .T. ) ;
#2402 = DIRECTION ( 'NONE',  ( -1.000000000000000000, 1.010728034814421376E-30, 1.090846720500930387E-30 ) ) ;
#2403 = ADVANCED_FACE ( 'NONE', ( #194 ), #6185, .T. ) ;
#2404 = EDGE_CURVE ( 'NONE', #9218, #291, #6309, .T. ) ;
#2405 = EDGE_CURVE ( 'NONE', #7451, #125, #4326, .T. ) ;
#2406 =( LENGTH_UNIT ( ) NAMED_UNIT ( * ) SI_UNIT ( .MILLI., .METRE. ) );
#2407 = AXIS2_PLACEMENT_3D ( 'NONE', #28, #11817, #3009 ) ;
#2408 = CIRCLE ( 'NONE', #3443, 2.149999999999992362 ) ;
#2409 = ORIENTED_EDGE ( 'NONE', *, *, #843, .F. ) ;
#2410 = LINE ( 'NONE', #11095, #4379 ) ;
#2411 = DIRECTION ( 'NONE',  ( -1.000000000000000000, 1.010728034814421376E-30, 1.090846720500930387E-30 ) ) ;
#2412 = DIRECTION ( 'NONE',  ( 0.000000000000000000, 0.000000000000000000, 1.000000000000000000 ) ) ;
#2413 = ADVANCED_FACE ( 'NONE', ( #4313 ), #12563, .F. ) ;
#2414 = CARTESIAN_POINT ( 'NONE',  ( 4.211140560182196069, 2.431303136016537358, -3.745885042887416638 ) ) ;
#2415 = CARTESIAN_POINT ( 'NONE',  ( -17.00000000000002842, -20.00000000000000000, 9.850000000000047606 ) ) ;
#2416 = PRODUCT_DEFINITION_FORMATION_WITH_SPECIFIED_SOURCE ( 'ANY', '', #6601, .NOT_KNOWN. ) ;
#2417 = AXIS2_PLACEMENT_3D ( 'NONE', #721, #847, #10566 ) ;
#2418 = LINE ( 'NONE', #7178, #11409 ) ;
#2419 = AXIS2_PLACEMENT_3D ( 'NONE', #11230, #2150, #2412 ) ;
#2420 = FACE_OUTER_BOUND ( 'NONE', #6608, .T. ) ;
#2421 = ORIENTED_EDGE ( 'NONE', *, *, #8953, .T. ) ;
#2422 = ORIENTED_EDGE ( 'NONE', *, *, #1157, .T. ) ;
#2423 = EDGE_LOOP ( 'NONE', ( #10077, #4368, #11891, #11402 ) ) ;
#2424 = ORIENTED_EDGE ( 'NONE', *, *, #6816, .F. ) ;
#2425 = SURFACE_SIDE_STYLE ('',( #10981 ) ) ;
#2426 = VECTOR ( 'NONE', #3154, 1000.000000000000000 ) ;
#2427 = DIRECTION ( 'NONE',  ( -2.465190328815656418E-32, 1.177425296209236734E-30, 1.000000000000000000 ) ) ;
#2428 = CARTESIAN_POINT ( 'NONE',  ( 20.00000000000000355, 19.99999999999999645, -12.00000000000000000 ) ) ;
#2429 = DIRECTION ( 'NONE',  ( -0.3420201433256680468, -7.946868433027813328E-32, 0.9396926207859086499 ) ) ;
#2430 = FACE_OUTER_BOUND ( 'NONE', #4109, .T. ) ;
#2431 = VERTEX_POINT ( 'NONE', #5279 ) ;
#2432 = EDGE_CURVE ( 'NONE', #8348, #4291, #385, .T. ) ;
#2433 = DIRECTION ( 'NONE',  ( -1.000000000000000000, -1.031065855027150586E-29, 2.218671295934095703E-30 ) ) ;
#2434 = DIRECTION ( 'NONE',  ( 0.000000000000000000, -1.000000000000000000, 0.000000000000000000 ) ) ;
#2435 = ORIENTED_EDGE ( 'NONE', *, *, #5855, .F. ) ;
#2436 = ORIENTED_EDGE ( 'NONE', *, *, #7161, .F. ) ;
#2437 = VERTEX_POINT ( 'NONE', #12311 ) ;
#2438 = ORIENTED_EDGE ( 'NONE', *, *, #10969, .T. ) ;
#2439 = EDGE_CURVE ( 'NONE', #8682, #11780, #6642, .T. ) ;
#2440 = CYLINDRICAL_SURFACE ( 'NONE', #3172, 2.800000000000003819 ) ;
#2441 = EDGE_CURVE ( 'NONE', #4499, #3985, #418, .T. ) ;
#2442 = CARTESIAN_POINT ( 'NONE',  ( -17.00000000000000000, 30.00000000000000000, 3.000000000000030198 ) ) ;
#2443 = ORIENTED_EDGE ( 'NONE', *, *, #6814, .F. ) ;
#2444 = FACE_OUTER_BOUND ( 'NONE', #7944, .T. ) ;
#2445 = EDGE_LOOP ( 'NONE', ( #8731, #6641 ) ) ;
#2446 = LINE ( 'NONE', #11331, #4270 ) ;
#2447 = FACE_OUTER_BOUND ( 'NONE', #1981, .T. ) ;
#2448 = VECTOR ( 'NONE', #8754, 1000.000000000000000 ) ;
#2449 = CARTESIAN_POINT ( 'NONE',  ( 19.99999999999999645, 5.025702764809077294, 5.431603052487407268 ) ) ;
#2450 = CARTESIAN_POINT ( 'NONE',  ( 0.000000000000000000, -4.518585619147925669, 5.860237538055052653 ) ) ;
#2451 = VERTEX_POINT ( 'NONE', #4642 ) ;
#2452 = ADVANCED_FACE ( 'NONE', ( #7596 ), #6376, .T. ) ;
#2453 = ORIENTED_EDGE ( 'NONE', *, *, #8794, .T. ) ;
#2454 = CARTESIAN_POINT ( 'NONE',  ( -16.99999999999999289, 30.00000000000000000, 25.00000000000007105 ) ) ;
#2455 = AXIS2_PLACEMENT_3D ( 'NONE', #12471, #3586, #7503 ) ;
#2456 = FILL_AREA_STYLE ('',( #8245 ) ) ;
#2457 = CARTESIAN_POINT ( 'NONE',  ( -4.197393957002295117, 0.4069871074557397939, -3.503767560748940468 ) ) ;
#2458 = DIRECTION ( 'NONE',  ( -1.000000000000000000, 6.162975822039154730E-33, 4.563833282352349791E-17 ) ) ;
#2459 = ADVANCED_FACE ( 'NONE', ( #8368 ), #5602, .T. ) ;
#2460 = AXIS2_PLACEMENT_3D ( 'NONE', #1881, #8829, #8955 ) ;
#2461 = AXIS2_PLACEMENT_3D ( 'NONE', #8419, #9369, #7579 ) ;
#2462 = CYLINDRICAL_SURFACE ( 'NONE', #6919, 2.800000000000003819 ) ;
#2463 = DIRECTION ( 'NONE',  ( 0.000000000000000000, 0.000000000000000000, 1.000000000000000000 ) ) ;
#2464 = CIRCLE ( 'NONE', #11085, 2.800000000000003819 ) ;
#2465 = FACE_OUTER_BOUND ( 'NONE', #10736, .T. ) ;
#2466 = EDGE_LOOP ( 'NONE', ( #12293, #4442 ) ) ;
#2467 = CARTESIAN_POINT ( 'NONE',  ( 4.000000000000001776, 2.309401076758487381, -3.433295621305364254 ) ) ;
#2468 = CARTESIAN_POINT ( 'NONE',  ( 21.00000000000003197, -30.00000000000000000, 5.000000000000011546 ) ) ;
#2469 = AXIS2_PLACEMENT_3D ( 'NONE', #3804, #11793, #6709 ) ;
#2470 = AXIS2_PLACEMENT_3D ( 'NONE', #3502, #528, #6590 ) ;
#2471 = CIRCLE ( 'NONE', #9640, 6.499000000000007660 ) ;
#2472 = VERTEX_POINT ( 'NONE', #2527 ) ;
#2473 = DIRECTION ( 'NONE',  ( -1.121661599611125110E-30, 0.9989930665413145894, 0.04486483035051865020 ) ) ;
#2474 = DIRECTION ( 'NONE',  ( -1.000000000000000000, 1.010728034814421376E-30, 1.090846720500930387E-30 ) ) ;
#2475 = LINE ( 'NONE', #10373, #2849 ) ;
#2476 = CARTESIAN_POINT ( 'NONE',  ( 14.00000000000000000, 30.00000000000000000, 6.000000000000000000 ) ) ;
#2477 = EDGE_CURVE ( 'NONE', #4568, #6306, #10550, .T. ) ;
#2478 = CARTESIAN_POINT ( 'NONE',  ( 19.99999999999997868, 5.914787828628611521, -4.446941076999673115 ) ) ;
#2479 = AXIS2_PLACEMENT_3D ( 'NONE', #7343, #3426, #3548 ) ;
#2480 = EDGE_CURVE ( 'NONE', #3728, #7005, #3105, .T. ) ;
#2481 = AXIS2_PLACEMENT_3D ( 'NONE', #7985, #6129, #6063 ) ;
#2482 = AXIS2_PLACEMENT_3D ( 'NONE', #3935, #3996, #1874 ) ;
#2483 = CARTESIAN_POINT ( 'NONE',  ( 40.00000000000000000, 39.49790820824818383, -24.06186359251417883 ) ) ;
#2484 = PRODUCT_DEFINITION_SHAPE ( 'NONE', 'NONE',  #5392 ) ;
#2485 = CARTESIAN_POINT ( 'NONE',  ( 0.000000000000000000, 4.163799117100989712E-16, -3.299999999999999822 ) ) ;
#2486 = ORIENTED_EDGE ( 'NONE', *, *, #8133, .T. ) ;
#2487 = CARTESIAN_POINT ( 'NONE',  ( 2.000000000000001776, -1.329782007511007169, 0.7677500000000010427 ) ) ;
#2488 = VERTEX_POINT ( 'NONE', #4511 ) ;
#2489 = VERTEX_POINT ( 'NONE', #1542 ) ;
#2490 = AXIS2_PLACEMENT_3D ( 'NONE', #11316, #1516, #5449 ) ;
#2491 = VERTEX_POINT ( 'NONE', #11473 ) ;
#2492 = EDGE_LOOP ( 'NONE', ( #5472, #2661, #6374, #990, #2581 ) ) ;
#2493 = CARTESIAN_POINT ( 'NONE',  ( -30.00000000000000000, -19.99999999999999645, 2.000000000000001776 ) ) ;
#2494 = DIRECTION ( 'NONE',  ( 0.000000000000000000, 0.000000000000000000, -1.000000000000000000 ) ) ;
#2495 = DIRECTION ( 'NONE',  ( 0.000000000000000000, 0.000000000000000000, -1.000000000000000000 ) ) ;
#2496 = DIRECTION ( 'NONE',  ( 0.000000000000000000, 0.000000000000000000, 1.000000000000000000 ) ) ;
#2497 = VERTEX_POINT ( 'NONE', #7348 ) ;
#2498 = CARTESIAN_POINT ( 'NONE',  ( 4.197393957002303999, -0.4069871074557490642, -3.503767560748930698 ) ) ;
#2499 = EDGE_CURVE ( 'NONE', #6983, #335, #11734, .T. ) ;
#2500 = FACE_OUTER_BOUND ( 'NONE', #3910, .T. ) ;
#2501 = ORIENTED_EDGE ( 'NONE', *, *, #10414, .T. ) ;
#2502 = ORIENTED_EDGE ( 'NONE', *, *, #1717, .T. ) ;
#2503 = ORIENTED_EDGE ( 'NONE', *, *, #6126, .T. ) ;
#2504 = ORIENTED_EDGE ( 'NONE', *, *, #6586, .T. ) ;
#2505 = LINE ( 'NONE', #5642, #4180 ) ;
#2506 = FACE_BOUND ( 'NONE', #463, .T. ) ;
#2507 = ORIENTED_EDGE ( 'NONE', *, *, #2018, .T. ) ;
#2508 = LINE ( 'NONE', #2712, #7385 ) ;
#2509 = DIRECTION ( 'NONE',  ( 0.000000000000000000, 0.000000000000000000, -1.000000000000000000 ) ) ;
#2510 = TOROIDAL_SURFACE ( 'NONE', #12586, 2.200000000000001066, 0.2000000000000000111 ) ;
#2511 = ORIENTED_EDGE ( 'NONE', *, *, #9481, .F. ) ;
#2512 = CARTESIAN_POINT ( 'NONE',  ( 14.00000000000000000, 49.63999999999998636, -5.000000000000001776 ) ) ;
#2513 = FACE_OUTER_BOUND ( 'NONE', #8088, .T. ) ;
#2514 = EDGE_CURVE ( 'NONE', #11904, #38, #10573, .T. ) ;
#2515 = DIRECTION ( 'NONE',  ( -1.000000000000000000, 1.010728034814421376E-30, 1.090846720500930387E-30 ) ) ;
#2516 = ADVANCED_FACE ( 'NONE', ( #2656 ), #624, .T. ) ;
#2517 = UNCERTAINTY_MEASURE_WITH_UNIT (LENGTH_MEASURE( 1.000000000000000082E-05 ), #10299, 'distance_accuracy_value', 'NONE');
#2518 = CIRCLE ( 'NONE', #9077, 1.610000000000000098 ) ;
#2519 = DIRECTION ( 'NONE',  ( -1.140150527077241873E-30, 0.000000000000000000, 1.000000000000000000 ) ) ;
#2520 = EDGE_CURVE ( 'NONE', #574, #12468, #4580, .T. ) ;
#2521 = ORIENTED_EDGE ( 'NONE', *, *, #5672, .F. ) ;
#2522 = CIRCLE ( 'NONE', #855, 4.000000000000008882 ) ;
#2523 = VERTEX_POINT ( 'NONE', #10424 ) ;
#2524 = DIRECTION ( 'NONE',  ( -1.238279320584846685E-16, 0.9554649393887558739, -0.2951046417778634412 ) ) ;
#2525 = ADVANCED_FACE ( 'NONE', ( #515 ), #7474, .T. ) ;
#2526 =( NAMED_UNIT ( * ) PLANE_ANGLE_UNIT ( ) SI_UNIT ( $, .RADIAN. ) );
#2527 = CARTESIAN_POINT ( 'NONE',  ( 0.000000000000000000, 6.146182963951664746, 2.112211157443887100 ) ) ;
#2528 = DIRECTION ( 'NONE',  ( -6.532754371361492628E-31, 0.9510565162951544194, -0.3090169943749445092 ) ) ;
#2529 = AXIS2_PLACEMENT_3D ( 'NONE', #11550, #2735, #9709 ) ;
#2530 = CARTESIAN_POINT ( 'NONE',  ( 19.99999999999999645, 7.380072687735807158, -0.5427035320837090282 ) ) ;
#2531 = CARTESIAN_POINT ( 'NONE',  ( 19.99999999999997868, 1.528443194675511707, -7.240432404259457222 ) ) ;
#2532 = CARTESIAN_POINT ( 'NONE',  ( 0.000000000000000000, 1.773042676681341856, -3.469446951953614189E-15 ) ) ;
#2533 = ORIENTED_EDGE ( 'NONE', *, *, #6615, .F. ) ;
#2534 = CARTESIAN_POINT ( 'NONE',  ( 0.6810597143199710324, 4.461075778259524505, -3.598441714920695311 ) ) ;
#2535 = AXIS2_PLACEMENT_3D ( 'NONE', #11358, #4653, #11486 ) ;
#2536 = DIRECTION ( 'NONE',  ( 1.000000000000000000, -1.010728034814421376E-30, -1.090846720500930387E-30 ) ) ;
#2537 = CIRCLE ( 'NONE', #2332, 6.000000000000000000 ) ;
#2538 = DIRECTION ( 'NONE',  ( 1.140150527077241873E-30, 0.000000000000000000, -1.000000000000000000 ) ) ;
#2539 = ORIENTED_EDGE ( 'NONE', *, *, #10803, .F. ) ;
#2540 = CARTESIAN_POINT ( 'NONE',  ( -9.000000000000000000, 49.63999999999998636, -13.00000000000000178 ) ) ;
#2541 = CYLINDRICAL_SURFACE ( 'NONE', #5422, 7.400000000000010125 ) ;
#2542 = AXIS2_PLACEMENT_3D ( 'NONE', #11966, #102, #1063 ) ;
#2543 = CARTESIAN_POINT ( 'NONE',  ( 14.00000000000000000, 61.31370849898475228, 3.999999999999997335 ) ) ;
#2544 = DIRECTION ( 'NONE',  ( 1.140150527077241873E-30, 0.000000000000000000, -1.000000000000000000 ) ) ;
#2545 = AXIS2_PLACEMENT_3D ( 'NONE', #1347, #9202, #386 ) ;
#2546 = CYLINDRICAL_SURFACE ( 'NONE', #3826, 7.400000000000010125 ) ;
#2547 = LINE ( 'NONE', #6468, #2790 ) ;
#2548 = DIRECTION ( 'NONE',  ( -1.000000000000000000, 1.006188713385347367E-17, 3.844790828812615713E-17 ) ) ;
#2549 = ORIENTED_EDGE ( 'NONE', *, *, #5470, .T. ) ;
#2550 = EDGE_CURVE ( 'NONE', #11042, #11825, #10490, .T. ) ;
#2551 = ORIENTED_EDGE ( 'NONE', *, *, #12161, .T. ) ;
#2552 = ORIENTED_EDGE ( 'NONE', *, *, #6765, .T. ) ;
#2553 = DIRECTION ( 'NONE',  ( -1.140150527077241873E-30, 0.000000000000000000, 1.000000000000000000 ) ) ;
#2554 = CARTESIAN_POINT ( 'NONE',  ( 20.00000000000000000, 16.59466514679920124, -6.965300083364789785 ) ) ;
#2555 = DIRECTION ( 'NONE',  ( 0.000000000000000000, 0.000000000000000000, 1.000000000000000000 ) ) ;
#2556 = DIRECTION ( 'NONE',  ( -1.000000000000000000, 1.010728034814421376E-30, 1.090846720500930387E-30 ) ) ;
#2557 = ORIENTED_EDGE ( 'NONE', *, *, #3685, .F. ) ;
#2558 = CARTESIAN_POINT ( 'NONE',  ( 33.00000000000001421, -6.037132280312101458E-17, -1.462922435963892052E-15 ) ) ;
#2559 = VECTOR ( 'NONE', #6363, 1000.000000000000000 ) ;
#2560 = CARTESIAN_POINT ( 'NONE',  ( -10.00000000000000178, 0.000000000000000000, 0.000000000000000000 ) ) ;
#2561 = ORIENTED_EDGE ( 'NONE', *, *, #1243, .T. ) ;
#2562 = ORIENTED_EDGE ( 'NONE', *, *, #5672, .T. ) ;
#2563 = DIRECTION ( 'NONE',  ( -1.000000000000000000, 1.010728034814421376E-30, 1.090846720500930387E-30 ) ) ;
#2564 = EDGE_LOOP ( 'NONE', ( #58, #5215 ) ) ;
#2565 = ORIENTED_EDGE ( 'NONE', *, *, #663, .F. ) ;
#2566 = VECTOR ( 'NONE', #3759, 1000.000000000000000 ) ;
#2567 = CARTESIAN_POINT ( 'NONE',  ( 4.000000000000019540, -2.309401076758522464, -3.433295621305367806 ) ) ;
#2568 = EDGE_CURVE ( 'NONE', #9520, #3892, #5407, .T. ) ;
#2569 = EDGE_CURVE ( 'NONE', #10994, #11920, #11947, .T. ) ;
#2570 = CIRCLE ( 'NONE', #4820, 3.500000000000000000 ) ;
#2571 = SURFACE_STYLE_FILL_AREA ( #10337 ) ;
#2572 = ORIENTED_EDGE ( 'NONE', *, *, #7361, .F. ) ;
#2573 = DIRECTION ( 'NONE',  ( 0.000000000000000000, 1.000000000000000000, 0.000000000000000000 ) ) ;
#2574 = CARTESIAN_POINT ( 'NONE',  ( 0.000000000000000000, -30.00000000000000000, 0.000000000000000000 ) ) ;
#2575 = VERTEX_POINT ( 'NONE', #2725 ) ;
#2576 = CARTESIAN_POINT ( 'NONE',  ( 0.000000000000000000, 0.000000000000000000, 0.000000000000000000 ) ) ;
#2577 = FACE_OUTER_BOUND ( 'NONE', #1203, .T. ) ;
#2578 = VECTOR ( 'NONE', #2994, 1000.000000000000000 ) ;
#2579 = DIRECTION ( 'NONE',  ( 0.000000000000000000, 0.000000000000000000, 1.000000000000000000 ) ) ;
#2580 = FACE_OUTER_BOUND ( 'NONE', #8850, .T. ) ;
#2581 = ORIENTED_EDGE ( 'NONE', *, *, #4127, .T. ) ;
#2582 = VERTEX_POINT ( 'NONE', #4698 ) ;
#2583 = PLANE ( 'NONE',  #11157 ) ;
#2584 = CIRCLE ( 'NONE', #9953, 7.400000000000009237 ) ;
#2585 = CARTESIAN_POINT ( 'NONE',  ( 29.00000000000006750, 3.469446951953614189E-15, -6.435967552322653956E-18 ) ) ;
#2586 = DIRECTION ( 'NONE',  ( -1.000000000000000000, 0.000000000000000000, 0.000000000000000000 ) ) ;
#2587 = LINE ( 'NONE', #642, #11771 ) ;
#2588 = PRODUCT ( 'spacer', 'spacer', '', ( #995 ) ) ;
#2589 = ADVANCED_FACE ( 'NONE', ( #9322 ), #8933, .T. ) ;
#2590 = LINE ( 'NONE', #10428, #4849 ) ;
#2591 = VECTOR ( 'NONE', #6970, 1000.000000000000000 ) ;
#2592 = CARTESIAN_POINT ( 'NONE',  ( -35.00000000000006395, -30.00000000000000000, 2.000000000000006661 ) ) ;
#2593 = ORIENTED_EDGE ( 'NONE', *, *, #4633, .T. ) ;
#2594 = DIRECTION ( 'NONE',  ( -1.000000000000000000, 1.010728034814421376E-30, 1.090846720500930387E-30 ) ) ;
#2595 = CARTESIAN_POINT ( 'NONE',  ( -15.00000000000000000, 30.00000000000000000, 3.000000000000029754 ) ) ;
#2596 = SURFACE_SIDE_STYLE ('',( #11353 ) ) ;
#2597 = EDGE_CURVE ( 'NONE', #4963, #9663, #954, .T. ) ;
#2598 = ADVANCED_FACE ( 'NONE', ( #7903 ), #5016, .F. ) ;
#2599 = DIRECTION ( 'NONE',  ( 0.000000000000000000, 0.000000000000000000, 1.000000000000000000 ) ) ;
#2600 = ORIENTED_EDGE ( 'NONE', *, *, #7623, .F. ) ;
#2601 = VECTOR ( 'NONE', #9717, 1000.000000000000000 ) ;
#2602 = FACE_OUTER_BOUND ( 'NONE', #12626, .T. ) ;
#2603 = COLOUR_RGB ( '', 0.31764706, 0.68627451, 0.89019608) ;
#2604 = CARTESIAN_POINT ( 'NONE',  ( 20.00000000000000355, 11.45997319858344810, -23.64547756539571566 ) ) ;
#2605 = DIRECTION ( 'NONE',  ( 1.000000000000000000, -1.010728034814421376E-30, -1.090846720500930387E-30 ) ) ;
#2606 = DIRECTION ( 'NONE',  ( -1.000000000000000000, -1.031065855027150586E-29, 2.218671295934095703E-30 ) ) ;
#2607 = DIRECTION ( 'NONE',  ( -1.000000000000000000, 1.010728034814421376E-30, 1.090846720500930387E-30 ) ) ;
#2608 = DIRECTION ( 'NONE',  ( -1.000000000000000000, 1.010728034814421376E-30, 1.090846720500930387E-30 ) ) ;
#2609 = UNCERTAINTY_MEASURE_WITH_UNIT (LENGTH_MEASURE( 1.000000000000000082E-05 ), #1825, 'distance_accuracy_value', 'NONE');
#2610 = VECTOR ( 'NONE', #10522, 1000.000000000000000 ) ;
#2611 = STYLED_ITEM ( 'NONE', ( #1255 ), #5784 ) ;
#2612 = DIRECTION ( 'NONE',  ( -1.454462294001238940E-30, 0.7227948638273878901, 0.6910626489868685329 ) ) ;
#2613 = ORIENTED_EDGE ( 'NONE', *, *, #9129, .T. ) ;
#2614 = ORIENTED_EDGE ( 'NONE', *, *, #1706, .F. ) ;
#2615 = ORIENTED_EDGE ( 'NONE', *, *, #4106, .T. ) ;
#2616 = EDGE_CURVE ( 'NONE', #7775, #10242, #10236, .T. ) ;
#2617 = DIRECTION ( 'NONE',  ( -1.000000000000000000, 1.224646799147356658E-16, 0.000000000000000000 ) ) ;
#2618 = DIRECTION ( 'NONE',  ( 1.000000000000000000, -0.000000000000000000, -0.000000000000000000 ) ) ;
#2619 = CARTESIAN_POINT ( 'NONE',  ( 0.000000000000000000, 3.565124043461679992, 5.527927226701645935 ) ) ;
#2620 = AXIS2_PLACEMENT_3D ( 'NONE', #9982, #7935, #1177 ) ;
#2621 = LINE ( 'NONE', #8341, #3639 ) ;
#2622 = EDGE_LOOP ( 'NONE', ( #8603, #1892, #8493, #4956 ) ) ;
#2623 = AXIS2_PLACEMENT_3D ( 'NONE', #10831, #7817, #5882 ) ;
#2624 = EDGE_CURVE ( 'NONE', #8729, #1807, #5914, .T. ) ;
#2625 = DIRECTION ( 'NONE',  ( -1.000000000000000000, 1.010728034814421376E-30, 1.090846720500930387E-30 ) ) ;
#2626 = DIRECTION ( 'NONE',  ( -9.737501798821852212E-31, 0.9909497617679352555, -0.1342332658176522697 ) ) ;
#2627 = ORIENTED_EDGE ( 'NONE', *, *, #5232, .T. ) ;
#2628 = ORIENTED_EDGE ( 'NONE', *, *, #5794, .T. ) ;
#2629 = CARTESIAN_POINT ( 'NONE',  ( 40.00000000000000711, 21.12780530657007816, -5.807015647486885257 ) ) ;
#2630 = EDGE_LOOP ( 'NONE', ( #457, #9132 ) ) ;
#2631 = AXIS2_PLACEMENT_3D ( 'NONE', #12157, #7255, #11177 ) ;
#2632 = ORIENTED_EDGE ( 'NONE', *, *, #5652, .F. ) ;
#2633 = AXIS2_PLACEMENT_3D ( 'NONE', #7982, #6909, #12060 ) ;
#2634 = CIRCLE ( 'NONE', #3256, 7.400000000000011902 ) ;
#2635 = FACE_BOUND ( 'NONE', #2445, .T. ) ;
#2636 = ORIENTED_EDGE ( 'NONE', *, *, #11706, .F. ) ;
#2637 = EDGE_CURVE ( 'NONE', #2127, #6031, #2789, .T. ) ;
#2638 = DIRECTION ( 'NONE',  ( -1.000000000000000000, 1.010728034814421376E-30, 1.090846720500930387E-30 ) ) ;
#2639 = DIRECTION ( 'NONE',  ( -1.000000000000000000, 1.010728034814421376E-30, 1.090846720500930387E-30 ) ) ;
#2640 = ORIENTED_EDGE ( 'NONE', *, *, #5125, .F. ) ;
#2641 = CARTESIAN_POINT ( 'NONE',  ( 1.317756351988344399, -3.857995168970216326, -0.04852650426602535261 ) ) ;
#2642 = DIRECTION ( 'NONE',  ( 0.000000000000000000, 0.000000000000000000, 1.000000000000000000 ) ) ;
#2643 = AXIS2_PLACEMENT_3D ( 'NONE', #9686, #4880, #11777 ) ;
#2644 = EDGE_CURVE ( 'NONE', #1822, #11190, #12694, .T. ) ;
#2645 = CARTESIAN_POINT ( 'NONE',  ( 19.99999999999999645, 5.362412286431453623, 3.809543717993933765 ) ) ;
#2646 = UNCERTAINTY_MEASURE_WITH_UNIT (LENGTH_MEASURE( 1.000000000000000082E-05 ), #12452, 'distance_accuracy_value', 'NONE');
#2647 = EDGE_CURVE ( 'NONE', #87, #2374, #2034, .T. ) ;
#2648 = FACE_BOUND ( 'NONE', #5059, .T. ) ;
#2649 = ADVANCED_FACE ( 'NONE', ( #8810 ), #3864, .T. ) ;
#2650 = ORIENTED_EDGE ( 'NONE', *, *, #7602, .T. ) ;
#2651 = ORIENTED_EDGE ( 'NONE', *, *, #448, .F. ) ;
#2652 =( REPRESENTATION_RELATIONSHIP ('NONE','NONE', #10018, #2726 ) REPRESENTATION_RELATIONSHIP_WITH_TRANSFORMATION ( #11110 )SHAPE_REPRESENTATION_RELATIONSHIP( ) );
#2653 = DIRECTION ( 'NONE',  ( -1.000000000000000000, 1.010728034814421376E-30, 1.090846720500930387E-30 ) ) ;
#2654 = DIRECTION ( 'NONE',  ( 1.000000000000000000, 0.000000000000000000, 0.000000000000000000 ) ) ;
#2655 = VERTEX_POINT ( 'NONE', #2049 ) ;
#2656 = FACE_OUTER_BOUND ( 'NONE', #1680, .T. ) ;
#2657 = CARTESIAN_POINT ( 'NONE',  ( 14.00000000000000000, 49.63999999999998636, -5.000000000000001776 ) ) ;
#2658 = DIRECTION ( 'NONE',  ( 0.000000000000000000, 0.7227948638273878901, 0.6910626489868685329 ) ) ;
#2659 = PRODUCT_DEFINITION ( 'UNKNOWN', '', #9190, #11796 ) ;
#2660 = DIRECTION ( 'NONE',  ( -1.000000000000000000, 1.010728034814421376E-30, 1.090846720500930387E-30 ) ) ;
#2661 = ORIENTED_EDGE ( 'NONE', *, *, #6635, .T. ) ;
#2662 = AXIS2_PLACEMENT_3D ( 'NONE', #5050, #3008, #4798 ) ;
#2663 = CARTESIAN_POINT ( 'NONE',  ( 9.000000000000017764, 19.99999999999999645, 14.15000000000002345 ) ) ;
#2664 = DIRECTION ( 'NONE',  ( -0.000000000000000000, -1.000000000000000000, -0.000000000000000000 ) ) ;
#2665 = PRESENTATION_STYLE_ASSIGNMENT (( #9584 ) ) ;
#2666 = EDGE_CURVE ( 'NONE', #4686, #11547, #11090, .T. ) ;
#2667 = CARTESIAN_POINT ( 'NONE',  ( 4.000000000000001776, 2.309401076758487381, -3.433295621305364254 ) ) ;
#2668 = ADVANCED_BREP_SHAPE_REPRESENTATION ( '', ( #10172, #12422 ), #7225 ) ;
#2669 = EDGE_CURVE ( 'NONE', #7265, #2754, #597, .T. ) ;
#2670 = CIRCLE ( 'NONE', #9827, 2.000000000000000888 ) ;
#2671 = VECTOR ( 'NONE', #10863, 1000.000000000000000 ) ;
#2672 = LINE ( 'NONE', #6394, #4168 ) ;
#2673 = CARTESIAN_POINT ( 'NONE',  ( 40.00000000000000711, 19.99999999999999645, -12.00000000000000178 ) ) ;
#2674 = CIRCLE ( 'NONE', #11508, 6.499000000000007660 ) ;
#2675 = CARTESIAN_POINT ( 'NONE',  ( 19.99999999999999645, -6.453973581750233279, -0.7636923504069568214 ) ) ;
#2676 = CARTESIAN_POINT ( 'NONE',  ( 11.17157287525379772, 30.00000000000000000, -2.828427124746177856 ) ) ;
#2677 = CARTESIAN_POINT ( 'NONE',  ( 0.000000000000000000, -6.310777386698704028, -1.552768423021405608 ) ) ;
#2678 = ADVANCED_FACE ( 'NONE', ( #890 ), #10614, .F. ) ;
#2679 = FACE_OUTER_BOUND ( 'NONE', #5687, .T. ) ;
#2680 = ADVANCED_FACE ( 'NONE', ( #9892 ), #1078, .T. ) ;
#2681 = CARTESIAN_POINT ( 'NONE',  ( 3.469446951953614189E-14, -3.469446951953614189E-15, -5.000000000000011546 ) ) ;
#2682 = AXIS2_PLACEMENT_3D ( 'NONE', #1610, #11414, #10295 ) ;
#2683 = PRESENTATION_LAYER_ASSIGNMENT (  '', '', ( #6367 ) ) ;
#2684 = DIRECTION ( 'NONE',  ( 7.272311470006191196E-31, 0.3513748240813435175, -0.9362348706397368714 ) ) ;
#2685 = ORIENTED_EDGE ( 'NONE', *, *, #9015, .F. ) ;
#2686 = AXIS2_PLACEMENT_3D ( 'NONE', #10737, #10986, #1923 ) ;
#2687 = EDGE_CURVE ( 'NONE', #363, #6740, #11718, .T. ) ;
#2688 = ORIENTED_EDGE ( 'NONE', *, *, #7898, .T. ) ;
#2689 = ORIENTED_EDGE ( 'NONE', *, *, #4520, .T. ) ;
#2690 = CARTESIAN_POINT ( 'NONE',  ( 5.384454397937153303, -3.469446951953614189E-15, -5.000000000000011546 ) ) ;
#2691 = VECTOR ( 'NONE', #5090, 1000.000000000000000 ) ;
#2692 = DIRECTION ( 'NONE',  ( -1.140150527077241873E-30, 0.000000000000000000, 1.000000000000000000 ) ) ;
#2693 = CARTESIAN_POINT ( 'NONE',  ( 33.00000000000001421, 81.84122341717352356, -2.681985084641642203 ) ) ;
#2694 = AXIS2_PLACEMENT_3D ( 'NONE', #203, #4132, #11745 ) ;
#2695 = VECTOR ( 'NONE', #1060, 1000.000000000000000 ) ;
#2696 = CYLINDRICAL_SURFACE ( 'NONE', #1359, 2.800000000000003819 ) ;
#2697 = EDGE_LOOP ( 'NONE', ( #5939, #9544, #4992, #8421 ) ) ;
#2698 = DIRECTION ( 'NONE',  ( 0.000000000000000000, 5.551115123125776539E-17, 1.000000000000000000 ) ) ;
#2699 = DIRECTION ( 'NONE',  ( -1.140150527077241873E-30, 0.000000000000000000, 1.000000000000000000 ) ) ;
#2700 = ORIENTED_EDGE ( 'NONE', *, *, #7431, .T. ) ;
#2701 = ORIENTED_EDGE ( 'NONE', *, *, #8073, .F. ) ;
#2702 = CARTESIAN_POINT ( 'NONE',  ( 19.99999999999999645, -1.268072931708538853, 6.374087545670210631 ) ) ;
#2703 = ORIENTED_EDGE ( 'NONE', *, *, #6258, .F. ) ;
#2704 = ORIENTED_EDGE ( 'NONE', *, *, #3659, .F. ) ;
#2705 = CIRCLE ( 'NONE', #7588, 1.610000000000000098 ) ;
#2706 = AXIS2_PLACEMENT_3D ( 'NONE', #8307, #8109, #2200 ) ;
#2707 = CARTESIAN_POINT ( 'NONE',  ( 15.00000000000003375, 12.50000000000000000, -4.062508476441825628E-31 ) ) ;
#2708 = ADVANCED_FACE ( 'NONE', ( #7848 ), #2977, .T. ) ;
#2709 = PRODUCT ( 'middle cover', 'middle cover', '', ( #4085 ) ) ;
#2710 = DIRECTION ( 'NONE',  ( 1.000000000000000000, 5.916456789157576279E-31, 0.000000000000000000 ) ) ;
#2711 = EDGE_LOOP ( 'NONE', ( #11837, #7268, #900, #4477 ) ) ;
#2712 = CARTESIAN_POINT ( 'NONE',  ( 40.00000000000000000, 39.34792583643766051, -14.91347054209568945 ) ) ;
#2713 = PLANE ( 'NONE',  #12131 ) ;
#2714 = ORIENTED_EDGE ( 'NONE', *, *, #1305, .F. ) ;
#2715 = CARTESIAN_POINT ( 'NONE',  ( -2.100000000000000089, -3.212271124132722995E-15, -0.2800830152838839626 ) ) ;
#2716 = CARTESIAN_POINT ( 'NONE',  ( 14.00000000000000000, -30.00000000000000000, 6.000000000000000000 ) ) ;
#2717 = MECHANICAL_DESIGN_GEOMETRIC_PRESENTATION_REPRESENTATION (  '', ( #4122 ), #5979 ) ;
#2718 = CARTESIAN_POINT ( 'NONE',  ( 19.99999999999999645, 0.000000000000000000, 0.000000000000000000 ) ) ;
#2719 = ORIENTED_EDGE ( 'NONE', *, *, #345, .F. ) ;
#2720 = ORIENTED_EDGE ( 'NONE', *, *, #840, .F. ) ;
#2721 = DIRECTION ( 'NONE',  ( 0.000000000000000000, 1.000000000000000000, 0.000000000000000000 ) ) ;
#2722 = DIRECTION ( 'NONE',  ( -6.073127713248504465E-17, 0.4837070886085645949, -0.8752299426035574648 ) ) ;
#2723 = ORIENTED_EDGE ( 'NONE', *, *, #3237, .T. ) ;
#2724 = EDGE_CURVE ( 'NONE', #4395, #4686, #10241, .T. ) ;
#2725 = CARTESIAN_POINT ( 'NONE',  ( 0.000000000000000000, 1.834336845376802971, -6.234758161925229913 ) ) ;
#2726 = SHAPE_REPRESENTATION ( 'ring', ( #12422 ), #20 ) ;
#2727 = ADVANCED_FACE ( 'NONE', ( #3355 ), #3168, .F. ) ;
#2728 = PLANE ( 'NONE',  #1850 ) ;
#2729 = FACE_OUTER_BOUND ( 'NONE', #11531, .T. ) ;
#2730 = AXIS2_PLACEMENT_3D ( 'NONE', #6143, #5187, #2022 ) ;
#2731 = DIRECTION ( 'NONE',  ( -1.000000000000000000, -1.031065855027150586E-29, 2.218671295934095703E-30 ) ) ;
#2732 = ORIENTED_EDGE ( 'NONE', *, *, #3539, .F. ) ;
#2733 = CARTESIAN_POINT ( 'NONE',  ( 19.99999999999999645, -6.289597356626462243, -3.898841506334609797 ) ) ;
#2734 = VERTEX_POINT ( 'NONE', #7273 ) ;
#2735 = DIRECTION ( 'NONE',  ( -1.224646799147352714E-16, -1.177425296209236909E-30, -1.000000000000000000 ) ) ;
#2736 =( NAMED_UNIT ( * ) SI_UNIT ( $, .STERADIAN. ) SOLID_ANGLE_UNIT ( ) );
#2737 = CARTESIAN_POINT ( 'NONE',  ( 0.000000000000000000, 5.956456411769424975, -2.790827096698929477 ) ) ;
#2738 = AXIS2_PLACEMENT_3D ( 'NONE', #4200, #4008, #1170 ) ;
#2739 = EDGE_CURVE ( 'NONE', #11576, #7570, #12107, .T. ) ;
#2740 = PRODUCT_DEFINITION ( 'UNKNOWN', '', #138, #12305 ) ;
#2741 = DIRECTION ( 'NONE',  ( 1.140150527077241873E-30, 0.000000000000000000, -1.000000000000000000 ) ) ;
#2742 = CARTESIAN_POINT ( 'NONE',  ( 0.000000000000000000, 0.000000000000000000, 0.000000000000000000 ) ) ;
#2743 = LINE ( 'NONE', #3571, #5501 ) ;
#2744 = DIRECTION ( 'NONE',  ( -1.000000000000000000, 1.010728034814421376E-30, 1.090846720500930387E-30 ) ) ;
#2745 = DIRECTION ( 'NONE',  ( 1.000000000000000000, 0.000000000000000000, 0.000000000000000000 ) ) ;
#2746 = CLOSED_SHELL ( 'NONE', ( #9617, #539, #4850, #4582, #5554, #3059, #5777, #10912, #10366, #6759, #10943, #2354, #1945, #996, #1209, #7851, #11352, #7779, #415, #8563, #6522, #11560 ) ) ;
#2747 = DIRECTION ( 'NONE',  ( -1.000000000000000000, 0.000000000000000000, 0.000000000000000000 ) ) ;
#2748 = AXIS2_PLACEMENT_3D ( 'NONE', #9007, #4121, #4055 ) ;
#2749 = DIRECTION ( 'NONE',  ( -1.000000000000000000, 1.010728034814421376E-30, 1.090846720500930387E-30 ) ) ;
#2750 = VERTEX_POINT ( 'NONE', #1271 ) ;
#2751 = EDGE_CURVE ( 'NONE', #11755, #9393, #12335, .T. ) ;
#2752 = ORIENTED_EDGE ( 'NONE', *, *, #7074, .T. ) ;
#2753 = ADVANCED_FACE ( 'NONE', ( #9951 ), #2317, .T. ) ;
#2754 = VERTEX_POINT ( 'NONE', #371 ) ;
#2755 = AXIS2_PLACEMENT_3D ( 'NONE', #8319, #3446, #4904 ) ;
#2756 = CARTESIAN_POINT ( 'NONE',  ( 0.000000000000000000, -6.484265599627161869, -1.105616797299001419 ) ) ;
#2757 = AXIS2_PLACEMENT_3D ( 'NONE', #11977, #10733, #4955 ) ;
#2758 = EDGE_CURVE ( 'NONE', #529, #9298, #10413, .T. ) ;
#2759 = CARTESIAN_POINT ( 'NONE',  ( 4.200000000000001954, 3.915468285211854230E-16, 2.200000000000003730 ) ) ;
#2760 = DIRECTION ( 'NONE',  ( 1.000000000000000000, -1.010728034814421376E-30, -1.090846720500930387E-30 ) ) ;
#2761 = CARTESIAN_POINT ( 'NONE',  ( 27.00000000000001421, -1.664003471950572653E-31, -1.232234986235134900E-15 ) ) ;
#2762 = VERTEX_POINT ( 'NONE', #6107 ) ;
#2763 = LINE ( 'NONE', #6677, #9550 ) ;
#2764 = ADVANCED_FACE ( 'NONE', ( #6233 ), #10017, .T. ) ;
#2765 = CARTESIAN_POINT ( 'NONE',  ( 19.99999999999999645, -0.4733669331952357062, 6.481737787550290619 ) ) ;
#2766 = ORIENTED_EDGE ( 'NONE', *, *, #12001, .T. ) ;
#2767 = AXIS2_PLACEMENT_3D ( 'NONE', #3149, #290, #4222 ) ;
#2768 = ORIENTED_EDGE ( 'NONE', *, *, #9825, .T. ) ;
#2769 = DIRECTION ( 'NONE',  ( -3.437775699846481192E-17, -0.2951046417778634967, -0.9554649393887558739 ) ) ;
#2770 = VERTEX_POINT ( 'NONE', #4043 ) ;
#2771 = VERTEX_POINT ( 'NONE', #10143 ) ;
#2772 = CARTESIAN_POINT ( 'NONE',  ( 0.000000000000000000, -4.357840574720623472, 4.821434073521961849 ) ) ;
#2773 = DIRECTION ( 'NONE',  ( 0.000000000000000000, 0.000000000000000000, 1.000000000000000000 ) ) ;
#2774 = EDGE_LOOP ( 'NONE', ( #6228, #9428, #5085 ) ) ;
#2775 = DIRECTION ( 'NONE',  ( -1.000000000000000000, 1.010728034814421376E-30, 1.090846720500930387E-30 ) ) ;
#2776 = EDGE_CURVE ( 'NONE', #11825, #1954, #1333, .T. ) ;
#2777 = DIRECTION ( 'NONE',  ( 0.000000000000000000, 0.000000000000000000, 1.000000000000000000 ) ) ;
#2778 = ORIENTED_EDGE ( 'NONE', *, *, #8111, .F. ) ;
#2779 = AXIS2_PLACEMENT_3D ( 'NONE', #84, #6070, #3950 ) ;
#2780 = DIRECTION ( 'NONE',  ( 1.000000000000000000, 0.000000000000000000, 0.000000000000000000 ) ) ;
#2781 = DIRECTION ( 'NONE',  ( -1.000000000000000000, 1.010728034814421376E-30, 1.090846720500930387E-30 ) ) ;
#2782 = VERTEX_POINT ( 'NONE', #5267 ) ;
#2783 = VERTEX_POINT ( 'NONE', #7967 ) ;
#2784 = AXIS2_PLACEMENT_3D ( 'NONE', #9956, #8166, #7338 ) ;
#2785 = ORIENTED_EDGE ( 'NONE', *, *, #8568, .T. ) ;
#2786 = DIRECTION ( 'NONE',  ( -1.000000000000000000, 1.010728034814421376E-30, 1.090846720500930387E-30 ) ) ;
#2787 = CARTESIAN_POINT ( 'NONE',  ( 14.99999999999999645, 39.34792583643766051, -17.06347054209567915 ) ) ;
#2788 = ORIENTED_EDGE ( 'NONE', *, *, #12668, .T. ) ;
#2789 = LINE ( 'NONE', #4767, #2671 ) ;
#2790 = VECTOR ( 'NONE', #12652, 1000.000000000000000 ) ;
#2791 = CARTESIAN_POINT ( 'NONE',  ( 15.00000000000003375, 12.50000000000000000, -4.062508476441825628E-31 ) ) ;
#2792 = EDGE_CURVE ( 'NONE', #10595, #4775, #12045, .T. ) ;
#2793 = CARTESIAN_POINT ( 'NONE',  ( 0.000000000000000000, 0.000000000000000000, 0.000000000000000000 ) ) ;
#2794 = CARTESIAN_POINT ( 'NONE',  ( -17.00000000000002842, -20.00000000000000000, 12.00000000000003730 ) ) ;
#2795 = ORIENTED_EDGE ( 'NONE', *, *, #2241, .F. ) ;
#2796 = CARTESIAN_POINT ( 'NONE',  ( 2.000000000000001776, 1.880445160090761061E-16, -1.535500000000000087 ) ) ;
#2797 = EDGE_LOOP ( 'NONE', ( #1927, #10870, #9691, #1870, #6527 ) ) ;
#2798 = AXIS2_PLACEMENT_3D ( 'NONE', #1194, #11778, #6822 ) ;
#2799 = LINE ( 'NONE', #8502, #12402 ) ;
#2800 = CARTESIAN_POINT ( 'NONE',  ( 40.00000000000000711, 10.64574963035789779, -21.19875926443459591 ) ) ;
#2801 = AXIS2_PLACEMENT_3D ( 'NONE', #10218, #9264, #3434 ) ;
#2802 = DIRECTION ( 'NONE',  ( 0.000000000000000000, 0.000000000000000000, 1.000000000000000000 ) ) ;
#2803 = DIRECTION ( 'NONE',  ( -1.000000000000000000, 1.010728034814421376E-30, 1.090846720500930387E-30 ) ) ;
#2805 = DIRECTION ( 'NONE',  ( 1.000000000000000000, 0.000000000000000000, -1.159061634649218351E-16 ) ) ;
#2804 = VECTOR ( 'NONE', #12374, 1000.000000000000114 ) ;
#2806 = CARTESIAN_POINT ( 'NONE',  ( 33.00000000000001421, 39.34792583643766761, -17.06347054209568270 ) ) ;
#2807 = AXIS2_PLACEMENT_3D ( 'NONE', #6219, #3406, #425 ) ;
#2808 = CARTESIAN_POINT ( 'NONE',  ( 4.200000000000001954, 1.110223024630118969E-16, 2.000000000000000888 ) ) ;
#2809 = DIRECTION ( 'NONE',  ( -0.7071067811865504593, 0.000000000000000000, -0.7071067811865445751 ) ) ;
#2810 = ADVANCED_FACE ( 'NONE', ( #8032 ), #11066, .T. ) ;
#2811 = EDGE_CURVE ( 'NONE', #3455, #4329, #11296, .T. ) ;
#2812 = CARTESIAN_POINT ( 'NONE',  ( -10.00000000000000178, 0.000000000000000000, 0.000000000000000000 ) ) ;
#2813 = ADVANCED_FACE ( 'NONE', ( #179 ), #9062, .T. ) ;
#2814 = EDGE_CURVE ( 'NONE', #6098, #3319, #6976, .T. ) ;
#2815 = DIRECTION ( 'NONE',  ( -1.000000000000000000, -1.031065855027150586E-29, 2.218671295934095703E-30 ) ) ;
#2816 = AXIS2_PLACEMENT_3D ( 'NONE', #3833, #7762, #12267 ) ;
#2817 = ORIENTED_EDGE ( 'NONE', *, *, #12561, .T. ) ;
#2818 = VERTEX_POINT ( 'NONE', #9125 ) ;
#2819 = LINE ( 'NONE', #1824, #8086 ) ;
#2820 = DIRECTION ( 'NONE',  ( -3.437775699846489820E-17, -0.2951046417778627751, -0.9554649393887560960 ) ) ;
#2821 = DIRECTION ( 'NONE',  ( 0.000000000000000000, 0.000000000000000000, -1.000000000000000000 ) ) ;
#2822 = DIRECTION ( 'NONE',  ( -1.000000000000000000, 1.010728034814421376E-30, 1.090846720500930387E-30 ) ) ;
#2823 = ORIENTED_EDGE ( 'NONE', *, *, #11411, .F. ) ;
#2824 = CARTESIAN_POINT ( 'NONE',  ( 0.000000000000000000, 7.358375340956995636, 0.7837807994561865055 ) ) ;
#2825 = APPLICATION_CONTEXT ( 'automotive_design' ) ;
#2826 = VECTOR ( 'NONE', #7333, 1000.000000000000000 ) ;
#2827 = CARTESIAN_POINT ( 'NONE',  ( 9.999999999999994671, -6.969736844459704095, 2.486517307195113879 ) ) ;
#2828 = VERTEX_POINT ( 'NONE', #3293 ) ;
#2829 = ORIENTED_EDGE ( 'NONE', *, *, #3369, .F. ) ;
#2830 = FACE_OUTER_BOUND ( 'NONE', #11061, .T. ) ;
#2831 = ORIENTED_EDGE ( 'NONE', *, *, #3749, .T. ) ;
#2832 = VERTEX_POINT ( 'NONE', #309 ) ;
#2833 = SURFACE_STYLE_FILL_AREA ( #1171 ) ;
#2834 = DIRECTION ( 'NONE',  ( -1.000000000000000000, 1.010728034814421376E-30, 1.090846720500930387E-30 ) ) ;
#2835 = ORIENTED_EDGE ( 'NONE', *, *, #11243, .T. ) ;
#2836 = AXIS2_PLACEMENT_3D ( 'NONE', #1110, #6982, #8059 ) ;
#2837 = CARTESIAN_POINT ( 'NONE',  ( 0.000000000000000000, 0.000000000000000000, 0.000000000000000000 ) ) ;
#2838 = EDGE_CURVE ( 'NONE', #3787, #35, #4750, .T. ) ;
#2839 = CIRCLE ( 'NONE', #11249, 2.149999999999999023 ) ;
#2840 = CARTESIAN_POINT ( 'NONE',  ( 50.00005079999998969, 5.204170427930421283E-15, -6.938893903907228378E-15 ) ) ;
#2841 = EDGE_LOOP ( 'NONE', ( #12665, #10276, #10719, #8806 ) ) ;
#2842 = DIRECTION ( 'NONE',  ( -1.000000000000000000, 1.010728034814421376E-30, 1.090846720500930387E-30 ) ) ;
#2843 = ADVANCED_FACE ( 'NONE', ( #1464, #2444 ), #5588, .T. ) ;
#2844 = FACE_OUTER_BOUND ( 'NONE', #9377, .T. ) ;
#2845 = PRODUCT_DEFINITION_FORMATION_WITH_SPECIFIED_SOURCE ( 'ANY', '', #724, .NOT_KNOWN. ) ;
#2846 = VECTOR ( 'NONE', #3387, 1000.000000000000000 ) ;
#2847 = ADVANCED_FACE ( 'NONE', ( #5394 ), #6357, .T. ) ;
#2848 = VERTEX_POINT ( 'NONE', #11392 ) ;
#2849 = VECTOR ( 'NONE', #4656, 1000.000000000000114 ) ;
#2850 = EDGE_CURVE ( 'NONE', #5717, #8530, #1444, .T. ) ;
#2851 = ORIENTED_EDGE ( 'NONE', *, *, #8169, .T. ) ;
#2852 = ORIENTED_EDGE ( 'NONE', *, *, #5325, .F. ) ;
#2853 = DIRECTION ( 'NONE',  ( -1.000000000000000000, 1.010728034814421376E-30, 1.090846720500930387E-30 ) ) ;
#2854 = ORIENTED_EDGE ( 'NONE', *, *, #10288, .F. ) ;
#2855 = CARTESIAN_POINT ( 'NONE',  ( 0.000000000000000000, 0.000000000000000000, 0.000000000000000000 ) ) ;
#2856 = ORIENTED_EDGE ( 'NONE', *, *, #3848, .F. ) ;
#2857 = CARTESIAN_POINT ( 'NONE',  ( 19.99999999999997868, 6.557268578288196537, 0.5199208220222073518 ) ) ;
#2858 = CARTESIAN_POINT ( 'NONE',  ( 0.5469614295418614436, -4.303013824935439047, -3.535263753545008658 ) ) ;
#2859 = CARTESIAN_POINT ( 'NONE',  ( 2.499999999999999556, -4.715201491944146941E-33, 3.469446951953614189E-15 ) ) ;
#2860 = ORIENTED_EDGE ( 'NONE', *, *, #9146, .F. ) ;
#2861 = DIRECTION ( 'NONE',  ( -1.000000000000000000, 1.010728034814421376E-30, 1.090846720500930387E-30 ) ) ;
#2862 = VERTEX_POINT ( 'NONE', #3540 ) ;
#2863 = CARTESIAN_POINT ( 'NONE',  ( 4.000000000000003553, 0.000000000000000000, -2.200000000000009504 ) ) ;
#2864 = EDGE_CURVE ( 'NONE', #9871, #1836, #1659, .T. ) ;
#2865 = CARTESIAN_POINT ( 'NONE',  ( 19.99999999999997868, 6.544726022087268724, -0.6592800351836389794 ) ) ;
#2866 = LINE ( 'NONE', #6847, #10925 ) ;
#2867 = CARTESIAN_POINT ( 'NONE',  ( 27.00000000000001066, 39.92642927056392210, -44.05727230799563898 ) ) ;
#2868 = LINE ( 'NONE', #7803, #5698 ) ;
#2869 = DIRECTION ( 'NONE',  ( 0.000000000000000000, 0.000000000000000000, 1.000000000000000000 ) ) ;
#2870 = CARTESIAN_POINT ( 'NONE',  ( 19.99999999999997868, 5.012092988314006625, -4.137139697483489087 ) ) ;
#2871 = CIRCLE ( 'NONE', #2455, 2.800000000000004263 ) ;
#2872 = FACE_BOUND ( 'NONE', #7830, .T. ) ;
#2873 = UNCERTAINTY_MEASURE_WITH_UNIT (LENGTH_MEASURE( 1.000000000000000082E-05 ), #11195, 'distance_accuracy_value', 'NONE');
#2874 = DIRECTION ( 'NONE',  ( -0.000000000000000000, -1.000000000000000000, 0.000000000000000000 ) ) ;
#2875 = PRESENTATION_LAYER_ASSIGNMENT (  '', '', ( #9631 ) ) ;
#2876 = EDGE_LOOP ( 'NONE', ( #4069, #1855, #2636, #1119 ) ) ;
#2877 = ORIENTED_EDGE ( 'NONE', *, *, #9073, .F. ) ;
#2878 = ADVANCED_FACE ( 'NONE', ( #688 ), #11522, .F. ) ;
#2879 = CARTESIAN_POINT ( 'NONE',  ( 19.99999999999999645, -0.1095571986795048497, 6.498076501567022767 ) ) ;
#2880 = CARTESIAN_POINT ( 'NONE',  ( 0.000000000000000000, 6.613766744932292774, -3.319350756341939324 ) ) ;
#2882 = EDGE_CURVE ( 'NONE', #7500, #4292, #10406, .T. ) ;
#2881 = CARTESIAN_POINT ( 'NONE',  ( 10.00000000000000178, 5.914787828628545796, 4.446941076999770814 ) ) ;
#2883 = LINE ( 'NONE', #5885, #749 ) ;
#2884 = VERTEX_POINT ( 'NONE', #6559 ) ;
#2885 = CARTESIAN_POINT ( 'NONE',  ( 19.99999999999999645, -6.486618105788068966, 0.4009819817179238743 ) ) ;
#2886 = CIRCLE ( 'NONE', #10042, 2.800000000000003819 ) ;
#2887 = VECTOR ( 'NONE', #1674, 1000.000000000000000 ) ;
#2888 = MECHANICAL_DESIGN_GEOMETRIC_PRESENTATION_REPRESENTATION (  '', ( #4724 ), #9029 ) ;
#2889 = CIRCLE ( 'NONE', #3294, 3.300000000000003375 ) ;
#2890 = FILL_AREA_STYLE ('',( #12540 ) ) ;
#2891 = ORIENTED_EDGE ( 'NONE', *, *, #323, .F. ) ;
#2892 = ORIENTED_EDGE ( 'NONE', *, *, #10410, .T. ) ;
#2893 = DIRECTION ( 'NONE',  ( 0.000000000000000000, 0.000000000000000000, 1.000000000000000000 ) ) ;
#2894 = ORIENTED_EDGE ( 'NONE', *, *, #12398, .T. ) ;
#2895 = ORIENTED_EDGE ( 'NONE', *, *, #9762, .T. ) ;
#2896 =( NAMED_UNIT ( * ) SI_UNIT ( $, .STERADIAN. ) SOLID_ANGLE_UNIT ( ) );
#2897 = AXIS2_PLACEMENT_3D ( 'NONE', #9255, #5155, #7153 ) ;
#2898 = DIRECTION ( 'NONE',  ( -1.000000000000000000, -1.081682119347366197E-16, 6.938893903907228378E-17 ) ) ;
#2899 = ORIENTED_EDGE ( 'NONE', *, *, #6245, .T. ) ;
#2900 = VECTOR ( 'NONE', #4591, 1000.000000000000000 ) ;
#2901 = CARTESIAN_POINT ( 'NONE',  ( 14.00000000000000000, -13.00000000000000000, 0.000000000000000000 ) ) ;
#2902 = DIRECTION ( 'NONE',  ( -1.848892746611746419E-31, -1.000000000000000000, 3.250006781153460502E-32 ) ) ;
#2903 = ORIENTED_EDGE ( 'NONE', *, *, #4894, .T. ) ;
#2904 = PRODUCT_DEFINITION ( 'UNKNOWN', '', #2416, #10936 ) ;
#2905 = FACE_OUTER_BOUND ( 'NONE', #11001, .T. ) ;
#2906 = APPLICATION_CONTEXT ( 'automotive_design' ) ;
#2907 = FACE_OUTER_BOUND ( 'NONE', #11846, .T. ) ;
#2908 = AXIS2_PLACEMENT_3D ( 'NONE', #635, #11400, #12375 ) ;
#2909 = AXIS2_PLACEMENT_3D ( 'NONE', #4053, #8942, #2927 ) ;
#2910 = VECTOR ( 'NONE', #10354, 1000.000000000000114 ) ;
#2911 = ORIENTED_EDGE ( 'NONE', *, *, #10731, .T. ) ;
#2912 = ORIENTED_EDGE ( 'NONE', *, *, #2597, .T. ) ;
#2913 = ORIENTED_EDGE ( 'NONE', *, *, #7561, .T. ) ;
#2914 = DIRECTION ( 'NONE',  ( 0.000000000000000000, -1.530455820933490821E-32, 1.000000000000000000 ) ) ;
#2915 = ORIENTED_EDGE ( 'NONE', *, *, #2244, .T. ) ;
#2916 = DIRECTION ( 'NONE',  ( 0.000000000000000000, 0.000000000000000000, 1.000000000000000000 ) ) ;
#2917 = VECTOR ( 'NONE', #9738, 1000.000000000000000 ) ;
#2918 = ORIENTED_EDGE ( 'NONE', *, *, #10760, .T. ) ;
#2919 = EDGE_CURVE ( 'NONE', #6872, #11175, #6360, .T. ) ;
#2920 = DIRECTION ( 'NONE',  ( -7.025792437124625182E-30, -0.4999999999999992784, 0.8660254037844390407 ) ) ;
#2921 = EDGE_CURVE ( 'NONE', #561, #2818, #5738, .T. ) ;
#2922 = ADVANCED_FACE ( 'NONE', ( #1592 ), #4625, .T. ) ;
#2923 = CARTESIAN_POINT ( 'NONE',  ( 9.999999999999994671, -6.413745496774120092, 3.691052519622234129 ) ) ;
#2924 = DIRECTION ( 'NONE',  ( -1.140150527077241873E-30, 0.000000000000000000, 1.000000000000000000 ) ) ;
#2925 = EDGE_CURVE ( 'NONE', #6318, #156, #7193, .T. ) ;
#2926 = ORIENTED_EDGE ( 'NONE', *, *, #1477, .F. ) ;
#2927 = DIRECTION ( 'NONE',  ( -1.000000000000000000, 0.000000000000000000, 0.000000000000000000 ) ) ;
#2928 = ORIENTED_EDGE ( 'NONE', *, *, #10118, .T. ) ;
#2929 = DIRECTION ( 'NONE',  ( -1.000000000000000000, 1.006188713385347367E-17, 3.844790828812615713E-17 ) ) ;
#2930 = LINE ( 'NONE', #72, #2065 ) ;
#2931 = LINE ( 'NONE', #10815, #5595 ) ;
#2932 = CIRCLE ( 'NONE', #2307, 1.610000000000001874 ) ;
#2933 = LINE ( 'NONE', #12587, #12088 ) ;
#2934 = CARTESIAN_POINT ( 'NONE',  ( 3.122502256758252770E-14, -4.618802153517027165, -3.433295621305388678 ) ) ;
#2935 = DIRECTION ( 'NONE',  ( 0.000000000000000000, -1.530455820933490821E-32, 1.000000000000000000 ) ) ;
#2936 = DIRECTION ( 'NONE',  ( -1.000000000000000000, -2.206481006425900381E-16, 8.674603474570138454E-17 ) ) ;
#2937 = CARTESIAN_POINT ( 'NONE',  ( 14.00000000000000000, 30.00000000000000000, 4.000000000000000000 ) ) ;
#2938 = AXIS2_PLACEMENT_3D ( 'NONE', #1031, #970, #8643 ) ;
#2939 = CARTESIAN_POINT ( 'NONE',  ( -4.000000000000022204, -1.344410693882025498E-14, -3.142992957459240344 ) ) ;
#2940 = AXIS2_PLACEMENT_3D ( 'NONE', #12319, #1488, #4519 ) ;
#2941 = VERTEX_POINT ( 'NONE', #5525 ) ;
#2942 = CARTESIAN_POINT ( 'NONE',  ( 19.99999999999997868, -0.9522442067290397549, -6.508557431545724192 ) ) ;
#2943 = DIRECTION ( 'NONE',  ( -0.000000000000000000, -1.000000000000000000, -0.000000000000000000 ) ) ;
#2944 = DIRECTION ( 'NONE',  ( 1.140150527077241873E-30, 0.000000000000000000, -1.000000000000000000 ) ) ;
#2945 = DIRECTION ( 'NONE',  ( -1.000000000000000000, 1.010728034814421376E-30, 1.090846720500930387E-30 ) ) ;
#2946 = DIRECTION ( 'NONE',  ( -1.000000000000000000, 1.010728034814421376E-30, 1.090846720500930387E-30 ) ) ;
#2947 = ORIENTED_EDGE ( 'NONE', *, *, #3112, .F. ) ;
#2948 = CARTESIAN_POINT ( 'NONE',  ( 19.99999999999997868, 6.557268578288196537, 3.319920822022211393 ) ) ;
#2949 = AXIS2_PLACEMENT_3D ( 'NONE', #7795, #1156, #8946 ) ;
#2950 = CARTESIAN_POINT ( 'NONE',  ( -35.00000000000006395, 19.99999999999999645, 2.000000000000007994 ) ) ;
#2951 = DIRECTION ( 'NONE',  ( 0.000000000000000000, -0.2951046417778627751, -0.9554649393887560960 ) ) ;
#2952 = ORIENTED_EDGE ( 'NONE', *, *, #3997, .T. ) ;
#2953 = ORIENTED_EDGE ( 'NONE', *, *, #9013, .F. ) ;
#2954 = EDGE_CURVE ( 'NONE', #8658, #7451, #8167, .T. ) ;
#2955 = CARTESIAN_POINT ( 'NONE',  ( 19.99999999999997868, 5.012092988314006625, -4.137139697483489087 ) ) ;
#2956 = ORIENTED_EDGE ( 'NONE', *, *, #2432, .T. ) ;
#2957 = VERTEX_POINT ( 'NONE', #12491 ) ;
#2958 = APPLICATION_PROTOCOL_DEFINITION ( 'draft international standard', 'automotive_design', 1998, #5265 ) ;
#2959 = VECTOR ( 'NONE', #366, 1000.000000000000000 ) ;
#2960 = DIRECTION ( 'NONE',  ( -1.000000000000000000, 1.010728034814421376E-30, 1.090846720500930387E-30 ) ) ;
#2961 = VERTEX_POINT ( 'NONE', #7336 ) ;
#2962 = FILL_AREA_STYLE_COLOUR ( '', #8420 ) ;
#2963 = PLANE ( 'NONE',  #12215 ) ;
#2964 = ORIENTED_EDGE ( 'NONE', *, *, #1708, .F. ) ;
#2965 = DIRECTION ( 'NONE',  ( -1.000000000000000000, -1.243449787580175168E-14, 0.000000000000000000 ) ) ;
#2966 = PLANE ( 'NONE',  #8734 ) ;
#2967 = AXIS2_PLACEMENT_3D ( 'NONE', #6544, #10387, #8398 ) ;
#2968 = ORIENTED_EDGE ( 'NONE', *, *, #9876, .F. ) ;
#2969 = EDGE_CURVE ( 'NONE', #4950, #11532, #3665, .T. ) ;
#2970 = ORIENTED_EDGE ( 'NONE', *, *, #1859, .T. ) ;
#2971 = EDGE_CURVE ( 'NONE', #4951, #5144, #4925, .T. ) ;
#2972 = ADVANCED_FACE ( 'NONE', ( #3602, #11458 ), #2713, .F. ) ;
#2973 = EDGE_LOOP ( 'NONE', ( #8784, #5135, #4932, #2593 ) ) ;
#2974 = DIRECTION ( 'NONE',  ( -1.000000000000000000, 0.000000000000000000, 0.000000000000000000 ) ) ;
#2975 = AXIS2_PLACEMENT_3D ( 'NONE', #6858, #10765, #792 ) ;
#2976 = ORIENTED_EDGE ( 'NONE', *, *, #4473, .T. ) ;
#2977 = CYLINDRICAL_SURFACE ( 'NONE', #7799, 6.499000000000010324 ) ;
#2978 = ORIENTED_EDGE ( 'NONE', *, *, #2187, .T. ) ;
#2979 = EDGE_CURVE ( 'NONE', #10149, #4676, #12299, .T. ) ;
#2980 = DIRECTION ( 'NONE',  ( 0.000000000000000000, 0.000000000000000000, 1.000000000000000000 ) ) ;
#2981 = AXIS2_PLACEMENT_3D ( 'NONE', #2867, #7614, #11554 ) ;
#2982 = DIRECTION ( 'NONE',  ( -0.5000000000000016653, 0.8660254037844378194, -1.094764425253763580E-47 ) ) ;
#2983 = ORIENTED_EDGE ( 'NONE', *, *, #4077, .T. ) ;
#2984 = DIRECTION ( 'NONE',  ( 0.000000000000000000, 0.000000000000000000, -1.000000000000000000 ) ) ;
#2985 = VERTEX_POINT ( 'NONE', #4688 ) ;
#2986 = DIRECTION ( 'NONE',  ( 0.000000000000000000, 0.000000000000000000, 1.000000000000000000 ) ) ;
#2987 = FILL_AREA_STYLE_COLOUR ( '', #2295 ) ;
#2988 = VECTOR ( 'NONE', #9468, 1000.000000000000000 ) ;
#2989 = DIRECTION ( 'NONE',  ( -1.000000000000000000, 1.010728034814421376E-30, 1.090846720500930387E-30 ) ) ;
#2990 = CARTESIAN_POINT ( 'NONE',  ( 2.000000000000001776, 1.773042676681338303, 0.000000000000000000 ) ) ;
#2991 = EDGE_CURVE ( 'NONE', #11641, #9518, #878, .T. ) ;
#2992 = DIRECTION ( 'NONE',  ( -1.000000000000000000, 1.010728034814421376E-30, 1.090846720500930387E-30 ) ) ;
#2993 = DIRECTION ( 'NONE',  ( 0.000000000000000000, 5.551115123125776539E-17, 1.000000000000000000 ) ) ;
#2994 = DIRECTION ( 'NONE',  ( -1.000000000000000000, 1.010728034814421376E-30, 1.090846720500930387E-30 ) ) ;
#2995 = AXIS2_PLACEMENT_3D ( 'NONE', #11807, #2935, #1814 ) ;
#2996 = CIRCLE ( 'NONE', #4631, 2.800000000000003819 ) ;
#2997 = DIRECTION ( 'NONE',  ( 1.140150527077241873E-30, 0.000000000000000000, -1.000000000000000000 ) ) ;
#2998 = CARTESIAN_POINT ( 'NONE',  ( 2.000000000000001776, 0.8865213383406622683, -1.535499999999995202 ) ) ;
#2999 = EDGE_CURVE ( 'NONE', #802, #10380, #8212, .T. ) ;
#3000 = LINE ( 'NONE', #7928, #10723 ) ;
#3001 = EDGE_CURVE ( 'NONE', #5017, #7234, #5712, .T. ) ;
#3002 = TOROIDAL_SURFACE ( 'NONE', #5451, 8.000000000000000000, 4.000000000000000000 ) ;
#3003 = ORIENTED_EDGE ( 'NONE', *, *, #4759, .F. ) ;
#3004 = AXIS2_PLACEMENT_3D ( 'NONE', #2558, #554, #5699 ) ;
#3005 = FACE_OUTER_BOUND ( 'NONE', #3654, .T. ) ;
#3006 = DIRECTION ( 'NONE',  ( 0.000000000000000000, 0.000000000000000000, 1.000000000000000000 ) ) ;
#3007 = FACE_OUTER_BOUND ( 'NONE', #1593, .T. ) ;
#3008 = DIRECTION ( 'NONE',  ( -1.000000000000000000, -1.081682119347366444E-16, 5.551115123125780237E-17 ) ) ;
#3009 = DIRECTION ( 'NONE',  ( 0.000000000000000000, 0.000000000000000000, 1.000000000000000000 ) ) ;
#3010 = VERTEX_POINT ( 'NONE', #3913 ) ;
#3011 = CARTESIAN_POINT ( 'NONE',  ( -17.00000000000002842, 19.99999999999998579, 12.00000000000003730 ) ) ;
#3012 = DIRECTION ( 'NONE',  ( -2.465190328815656418E-32, 1.177425296209236734E-30, 1.000000000000000000 ) ) ;
#3013 = CARTESIAN_POINT ( 'NONE',  ( -7.888106377466153063, 30.00000000000000000, -1.333333333333333703 ) ) ;
#3014 = ORIENTED_EDGE ( 'NONE', *, *, #4338, .F. ) ;
#3015 = AXIS2_PLACEMENT_3D ( 'NONE', #2222, #10051, #10116 ) ;
#3016 = ORIENTED_EDGE ( 'NONE', *, *, #925, .F. ) ;
#3017 = CYLINDRICAL_SURFACE ( 'NONE', #4567, 6.499000000000010324 ) ;
#3018 = ORIENTED_EDGE ( 'NONE', *, *, #3041, .T. ) ;
#3019 = VERTEX_POINT ( 'NONE', #1970 ) ;
#3020 = SHAPE_DEFINITION_REPRESENTATION ( #9140, #10018 ) ;
#3021 = ADVANCED_FACE ( 'NONE', ( #11584 ), #8739, .F. ) ;
#3022 = DIRECTION ( 'NONE',  ( -1.848892746611746419E-31, -1.000000000000000000, 3.250006781153460502E-32 ) ) ;
#3023 = VERTEX_POINT ( 'NONE', #12618 ) ;
#3024 = DIRECTION ( 'NONE',  ( -1.000000000000000000, -1.081682119347366197E-16, 6.938893903907228378E-17 ) ) ;
#3025 = EDGE_CURVE ( 'NONE', #4994, #7580, #2570, .T. ) ;
#3026 = DIRECTION ( 'NONE',  ( 0.000000000000000000, 1.000000000000000000, 0.000000000000000000 ) ) ;
#3027 = ORIENTED_EDGE ( 'NONE', *, *, #2241, .T. ) ;
#3028 = CARTESIAN_POINT ( 'NONE',  ( 40.00000000000000711, 19.99999999999999645, -9.850000000000010303 ) ) ;
#3029 = AXIS2_PLACEMENT_3D ( 'NONE', #9184, #5082, #3166 ) ;
#3030 = DIRECTION ( 'NONE',  ( 1.084202172485504434E-16, 0.000000000000000000, 1.000000000000000000 ) ) ;
#3031 = ORIENTED_EDGE ( 'NONE', *, *, #10270, .F. ) ;
#3032 = ORIENTED_EDGE ( 'NONE', *, *, #5231, .T. ) ;
#3033 = ORIENTED_EDGE ( 'NONE', *, *, #11401, .T. ) ;
#3034 = ADVANCED_FACE ( 'NONE', ( #4755 ), #5902, .T. ) ;
#3035 = CARTESIAN_POINT ( 'NONE',  ( -3.999999999999991562, 2.309401076758501592, -4.999999999999993783 ) ) ;
#3036 = CIRCLE ( 'NONE', #12077, 2.800000000000004263 ) ;
#3037 = ORIENTED_EDGE ( 'NONE', *, *, #2647, .T. ) ;
#3038 = DIRECTION ( 'NONE',  ( 1.000000000000000000, 1.081682119347366321E-16, -6.938893903907228378E-17 ) ) ;
#3039 = EDGE_LOOP ( 'NONE', ( #6750, #11892, #8395, #9336 ) ) ;
#3040 = EDGE_CURVE ( 'NONE', #5879, #8571, #4201, .T. ) ;
#3041 = EDGE_CURVE ( 'NONE', #144, #1272, #5845, .T. ) ;
#3042 = AXIS2_PLACEMENT_3D ( 'NONE', #3819, #3939, #6595 ) ;
#3043 = EDGE_CURVE ( 'NONE', #3101, #7946, #1848, .T. ) ;
#3044 = VECTOR ( 'NONE', #5677, 1000.000000000000000 ) ;
#3045 = CYLINDRICAL_SURFACE ( 'NONE', #8943, 6.499000000000010324 ) ;
#3046 = CARTESIAN_POINT ( 'NONE',  ( 0.000000000000000000, -4.518585619147845733, -5.860237538055125484 ) ) ;
#3047 = VERTEX_POINT ( 'NONE', #7774 ) ;
#3048 = LINE ( 'NONE', #6771, #1004 ) ;
#3049 = ORIENTED_EDGE ( 'NONE', *, *, #10659, .T. ) ;
#3050 = CYLINDRICAL_SURFACE ( 'NONE', #12197, 24.99999999999999289 ) ;
#3051 = DIRECTION ( 'NONE',  ( 0.000000000000000000, 0.000000000000000000, 1.000000000000000000 ) ) ;
#3052 = CARTESIAN_POINT ( 'NONE',  ( -29.99999999999999289, -30.00000000000000000, 1.672083814130525448E-15 ) ) ;
#3053 = DIRECTION ( 'NONE',  ( 1.000000000000000000, -1.010728034814421376E-30, -1.090846720500930387E-30 ) ) ;
#3054 = EDGE_CURVE ( 'NONE', #803, #11695, #6235, .T. ) ;
#3055 = DIRECTION ( 'NONE',  ( -1.000000000000000000, 1.010728034814421376E-30, 1.090846720500930387E-30 ) ) ;
#3056 = DIRECTION ( 'NONE',  ( -1.000000000000000000, 1.010728034814421376E-30, 1.090846720500930387E-30 ) ) ;
#3057 = DIRECTION ( 'NONE',  ( 0.000000000000000000, 1.000000000000000000, -1.224646799147353207E-16 ) ) ;
#3058 = DIRECTION ( 'NONE',  ( -4.930380657631325535E-31, -1.000000000000000000, -1.177425296209239362E-30 ) ) ;
#3059 = ADVANCED_FACE ( 'NONE', ( #8608 ), #9684, .F. ) ;
#3060 = CARTESIAN_POINT ( 'NONE',  ( 0.000000000000000000, -4.357840574720561300, -4.821434073522038233 ) ) ;
#3061 = APPLICATION_CONTEXT ( 'automotive_design' ) ;
#3062 = ORIENTED_EDGE ( 'NONE', *, *, #6963, .T. ) ;
#3063 = ORIENTED_EDGE ( 'NONE', *, *, #6754, .T. ) ;
#3064 = LINE ( 'NONE', #10110, #3788 ) ;
#3065 = LINE ( 'NONE', #5818, #4502 ) ;
#3066 = ADVANCED_FACE ( 'NONE', ( #6819 ), #2963, .F. ) ;
#3067 = CARTESIAN_POINT ( 'NONE',  ( 0.000000000000000000, -0.9522442067290397549, -6.508557431545724192 ) ) ;
#3068 = ORIENTED_EDGE ( 'NONE', *, *, #4877, .T. ) ;
#3069 = DIRECTION ( 'NONE',  ( -1.000000000000000000, -1.031065855027150586E-29, 2.218671295934095703E-30 ) ) ;
#3070 = EDGE_CURVE ( 'NONE', #3108, #11779, #5837, .T. ) ;
#3071 = CARTESIAN_POINT ( 'NONE',  ( 0.000000000000000000, -30.00000000000000000, -9.999999999999998224 ) ) ;
#3072 = LINE ( 'NONE', #10904, #2257 ) ;
#3073 = ORIENTED_EDGE ( 'NONE', *, *, #1665, .F. ) ;
#3074 = ORIENTED_EDGE ( 'NONE', *, *, #11077, .F. ) ;
#3075 = EDGE_CURVE ( 'NONE', #3964, #2374, #942, .T. ) ;
#3076 = DIRECTION ( 'NONE',  ( 1.000000000000000000, 1.849040895279789448E-31, -6.938893903907224680E-17 ) ) ;
#3077 = ORIENTED_EDGE ( 'NONE', *, *, #10381, .F. ) ;
#3078 = CIRCLE ( 'NONE', #10230, 2.800000000000002931 ) ;
#3079 = VERTEX_POINT ( 'NONE', #8800 ) ;
#3080 = APPLICATION_PROTOCOL_DEFINITION ( 'draft international standard', 'automotive_design', 1998, #5674 ) ;
#3081 = CARTESIAN_POINT ( 'NONE',  ( 13.63191942669736889, 30.00000000000001776, 3.758770483143646146 ) ) ;
#3082 = VERTEX_POINT ( 'NONE', #10788 ) ;
#3083 = CARTESIAN_POINT ( 'NONE',  ( 9.999999999999998224, -30.00000000000000000, -6.123233995736765296E-16 ) ) ;
#3084 = DIRECTION ( 'NONE',  ( 0.000000000000000000, -1.000000000000000000, 0.000000000000000000 ) ) ;
#3085 = ORIENTED_EDGE ( 'NONE', *, *, #6575, .T. ) ;
#3086 = CIRCLE ( 'NONE', #5562, 7.400000000000011902 ) ;
#3087 = AXIS2_PLACEMENT_3D ( 'NONE', #11131, #4300, #8164 ) ;
#3088 = CARTESIAN_POINT ( 'NONE',  ( 40.00000000000000000, 39.34792583643766051, -17.06347054209567915 ) ) ;
#3089 = LINE ( 'NONE', #6029, #6704 ) ;
#3090 = VECTOR ( 'NONE', #5249, 1000.000000000000000 ) ;
#3091 = EDGE_LOOP ( 'NONE', ( #11028, #9675, #7446, #2915 ) ) ;
#3092 = ORIENTED_EDGE ( 'NONE', *, *, #4506, .T. ) ;
#3093 = CIRCLE ( 'NONE', #3700, 2.800000000000003819 ) ;
#3094 = ORIENTED_EDGE ( 'NONE', *, *, #3425, .T. ) ;
#3095 = AXIS2_PLACEMENT_3D ( 'NONE', #12653, #9721, #11431 ) ;
#3096 = CIRCLE ( 'NONE', #812, 7.400000000000011902 ) ;
#3097 = CARTESIAN_POINT ( 'NONE',  ( 9.999999999999994671, -7.258495115966583811, 1.440225208600806717 ) ) ;
#3098 = CARTESIAN_POINT ( 'NONE',  ( 19.99999999999997868, -3.399584271718297579, -6.572885726945642659 ) ) ;
#3099 = EDGE_LOOP ( 'NONE', ( #7832, #5555, #8417, #6841, #4080 ) ) ;
#3100 = CARTESIAN_POINT ( 'NONE',  ( 4.000000000000000888, 1.563622288139203453, -0.2253451193528330232 ) ) ;
#3101 = VERTEX_POINT ( 'NONE', #752 ) ;
#3102 = DIRECTION ( 'NONE',  ( -1.000000000000000000, 1.010728034814421376E-30, 1.090846720500930387E-30 ) ) ;
#3103 = CIRCLE ( 'NONE', #11936, 6.000000000000000000 ) ;
#3104 = AXIS2_PLACEMENT_3D ( 'NONE', #5289, #11155, #11282 ) ;
#3105 = CIRCLE ( 'NONE', #4536, 9.999999999999998224 ) ;
#3106 = CARTESIAN_POINT ( 'NONE',  ( 4.175648173966059140, -2.207990556236545832, -3.469390959564068400 ) ) ;
#3107 = DIRECTION ( 'NONE',  ( 0.000000000000000000, 0.4999999999999989453, -0.8660254037844392627 ) ) ;
#3108 = VERTEX_POINT ( 'NONE', #7649 ) ;
#3109 = CARTESIAN_POINT ( 'NONE',  ( 4.211140560182196069, 2.431303136016537358, -3.745885042887416638 ) ) ;
#3110 = EDGE_LOOP ( 'NONE', ( #11693, #9803, #12735, #1781 ) ) ;
#3111 = FACE_OUTER_BOUND ( 'NONE', #10549, .T. ) ;
#3112 = EDGE_CURVE ( 'NONE', #3412, #8231, #3727, .T. ) ;
#3113 =( GEOMETRIC_REPRESENTATION_CONTEXT ( 3 ) GLOBAL_UNCERTAINTY_ASSIGNED_CONTEXT ( ( #10448 ) ) GLOBAL_UNIT_ASSIGNED_CONTEXT ( ( #6131, #3843, #12064 ) ) REPRESENTATION_CONTEXT ( 'NONE', 'WORKASPACE' ) );
#3114 = CIRCLE ( 'NONE', #11322, 6.499000000000008548 ) ;
#3115 = FACE_OUTER_BOUND ( 'NONE', #879, .T. ) ;
#3116 = DIRECTION ( 'NONE',  ( 0.000000000000000000, 0.000000000000000000, 1.000000000000000000 ) ) ;
#3117 = DIRECTION ( 'NONE',  ( -1.000000000000000000, 1.010728034814421376E-30, 1.090846720500930387E-30 ) ) ;
#3118 = DIRECTION ( 'NONE',  ( 0.000000000000000000, -1.000000000000000000, 0.000000000000000000 ) ) ;
#3119 =( GEOMETRIC_REPRESENTATION_CONTEXT ( 3 ) GLOBAL_UNCERTAINTY_ASSIGNED_CONTEXT ( ( #694 ) ) GLOBAL_UNIT_ASSIGNED_CONTEXT ( ( #1092, #193, #1994 ) ) REPRESENTATION_CONTEXT ( 'NONE', 'WORKASPACE' ) );
#3120 = CARTESIAN_POINT ( 'NONE',  ( -4.211140560182161430, -2.431303136016561783, -3.745885042887451277 ) ) ;
#3121 = CARTESIAN_POINT ( 'NONE',  ( 3.469446951953614189E-14, -3.469446951953614189E-15, -4.694516984716123886 ) ) ;
#3122 = CARTESIAN_POINT ( 'NONE',  ( 19.99999999999999645, -5.148708580507647348, -3.965829163366334953 ) ) ;
#3123 = ADVANCED_FACE ( 'NONE', ( #4941 ), #44, .T. ) ;
#3124 = SURFACE_SIDE_STYLE ('',( #2833 ) ) ;
#3125 = VECTOR ( 'NONE', #11827, 1000.000000000000000 ) ;
#3126 = ORIENTED_EDGE ( 'NONE', *, *, #2724, .T. ) ;
#3127 = CARTESIAN_POINT ( 'NONE',  ( 33.00000000000000711, 39.92642927056392210, -24.05727230799563898 ) ) ;
#3128 = FACE_OUTER_BOUND ( 'NONE', #11826, .T. ) ;
#3129 =( BOUNDED_SURFACE ( )  B_SPLINE_SURFACE ( 3, 2, ( 
 ( #6896, #12699, #9826 ),
 ( #7733, #2858, #1022 ),
 ( #8628, #6835, #833 ),
 ( #3744, #1274, #5021 ),
 ( #376, #314, #6238 ),
 ( #3106, #2254, #9895 ) ),
 .UNSPECIFIED., .F., .F., .F. ) 
 B_SPLINE_SURFACE_WITH_KNOTS ( ( 4, 2, 4 ),
 ( 3, 3 ),
 ( 0.02032853247518126918, 0.02278863295364821906, 0.02524873343211517240 ),
 ( 0.000000000000000000, 1.000000000000000000 ),
 .UNSPECIFIED. ) 
 GEOMETRIC_REPRESENTATION_ITEM ( )  RATIONAL_B_SPLINE_SURFACE ( (
 ( 1.000000000000000000, 0.8047781615896836271, 1.000000000000000000),
 ( 1.000000000000000000, 0.8123767586288546116, 1.000000000000000000),
 ( 1.000000000000000000, 0.8190662415565334031, 1.000000000000000000),
 ( 1.000000000000000000, 0.8192361015668073732, 1.000000000000000000),
 ( 1.000000000000000000, 0.8126135807104617470, 1.000000000000000000),
 ( 1.000000000000000000, 0.8047712338318590009, 1.000000000000000000) ) ) 
 REPRESENTATION_ITEM ( '' )  SURFACE ( )  );
#3130 = CARTESIAN_POINT ( 'NONE',  ( 19.99999999999997868, 6.557268578288196537, 0.5199208220222073518 ) ) ;
#3131 = FACE_OUTER_BOUND ( 'NONE', #3091, .T. ) ;
#3132 = EDGE_CURVE ( 'NONE', #10380, #8069, #5210, .T. ) ;
#3133 = CARTESIAN_POINT ( 'NONE',  ( 9.999999999999998224, 5.200656487704272912, 5.264330166022994639 ) ) ;
#3134 = ORIENTED_EDGE ( 'NONE', *, *, #7001, .F. ) ;
#3135 = CARTESIAN_POINT ( 'NONE',  ( 28.61000000000001009, 1.339070573674431444E-16, -2.000000000000001332 ) ) ;
#3136 = CIRCLE ( 'NONE', #4179, 4.000000000000008882 ) ;
#3137 = DIRECTION ( 'NONE',  ( 0.000000000000000000, -0.9749279121818259508, 0.2225209339563041233 ) ) ;
#3138 = VECTOR ( 'NONE', #2664, 1000.000000000000000 ) ;
#3139 = DIRECTION ( 'NONE',  ( 1.238279320584846685E-16, -0.9554649393887560960, 0.2951046417778627751 ) ) ;
#3140 = EDGE_CURVE ( 'NONE', #11532, #10836, #10744, .T. ) ;
#3141 = ORIENTED_EDGE ( 'NONE', *, *, #7277, .T. ) ;
#3142 = DIRECTION ( 'NONE',  ( 0.000000000000000000, 0.000000000000000000, -1.000000000000000000 ) ) ;
#3143 = ORIENTED_EDGE ( 'NONE', *, *, #5646, .T. ) ;
#3144 = ORIENTED_EDGE ( 'NONE', *, *, #838, .F. ) ;
#3145 = EDGE_CURVE ( 'NONE', #7082, #509, #5966, .T. ) ;
#3146 = EDGE_CURVE ( 'NONE', #6793, #5973, #10124, .T. ) ;
#3147 = CARTESIAN_POINT ( 'NONE',  ( 19.99999999999997868, 6.359055127044406674, -1.682410996215896848 ) ) ;
#3148 = ORIENTED_EDGE ( 'NONE', *, *, #8827, .F. ) ;
#3149 = CARTESIAN_POINT ( 'NONE',  ( 0.000000000000000000, 6.557268578288212524, -0.5199208220221240850 ) ) ;
#3150 = AXIS2_PLACEMENT_3D ( 'NONE', #7284, #321, #2393 ) ;
#3151 = EDGE_LOOP ( 'NONE', ( #12169, #9101, #10311, #1178, #8918 ) ) ;
#3152 = DIRECTION ( 'NONE',  ( 0.000000000000000000, 0.000000000000000000, 1.000000000000000000 ) ) ;
#3153 = DIRECTION ( 'NONE',  ( -3.437775699846489820E-17, -0.2951046417778627751, -0.9554649393887560960 ) ) ;
#3154 = DIRECTION ( 'NONE',  ( -0.000000000000000000, -1.000000000000000000, -0.000000000000000000 ) ) ;
#3155 = EDGE_CURVE ( 'NONE', #7064, #12067, #7680, .T. ) ;
#3156 = CARTESIAN_POINT ( 'NONE',  ( 9.000000000000017764, 19.99999999999999645, 12.00000000000003020 ) ) ;
#3157 = ORIENTED_EDGE ( 'NONE', *, *, #2882, .T. ) ;
#3158 = ORIENTED_EDGE ( 'NONE', *, *, #8084, .T. ) ;
#3159 = VECTOR ( 'NONE', #10958, 1000.000000000000000 ) ;
#3160 = VERTEX_POINT ( 'NONE', #228 ) ;
#3161 = AXIS2_PLACEMENT_3D ( 'NONE', #1794, #1538, #6639 ) ;
#3162 = ORIENTED_EDGE ( 'NONE', *, *, #1839, .T. ) ;
#3163 = EDGE_CURVE ( 'NONE', #4169, #3964, #68, .T. ) ;
#3164 = DIRECTION ( 'NONE',  ( 0.000000000000000000, 0.5128992774059070170, -0.8584487936018656562 ) ) ;
#3165 = ADVANCED_FACE ( 'NONE', ( #7955 ), #7004, .T. ) ;
#3166 = DIRECTION ( 'NONE',  ( 8.135128085091671982E-31, 0.1785568947986369281, -0.9839295885986296675 ) ) ;
#3167 = ORIENTED_EDGE ( 'NONE', *, *, #12083, .F. ) ;
#3168 = PLANE ( 'NONE',  #3087 ) ;
#3169 = VERTEX_POINT ( 'NONE', #3337 ) ;
#3170 = AXIS2_PLACEMENT_3D ( 'NONE', #605, #11373, #2553 ) ;
#3171 = DIRECTION ( 'NONE',  ( -1.000000000000000000, 1.010728034814421376E-30, 1.090846720500930387E-30 ) ) ;
#3172 = AXIS2_PLACEMENT_3D ( 'NONE', #9058, #4362, #6166 ) ;
#3173 = DIRECTION ( 'NONE',  ( -1.000000000000000000, 1.010728034814421376E-30, 1.090846720500930387E-30 ) ) ;
#3174 = DIRECTION ( 'NONE',  ( 0.000000000000000000, 1.000000000000000000, 0.000000000000000000 ) ) ;
#3175 = ORIENTED_EDGE ( 'NONE', *, *, #12697, .T. ) ;
#3176 = LINE ( 'NONE', #5517, #3290 ) ;
#3177 = CIRCLE ( 'NONE', #5625, 7.999999999999998224 ) ;
#3178 = VERTEX_POINT ( 'NONE', #9110 ) ;
#3179 = CARTESIAN_POINT ( 'NONE',  ( 0.000000000000000000, -1.113123845672308709, -7.315801754025043735 ) ) ;
#3180 = EDGE_CURVE ( 'NONE', #12656, #4412, #8699, .T. ) ;
#3181 = DIRECTION ( 'NONE',  ( 0.000000000000000000, 0.4999999999999989453, -0.8660254037844392627 ) ) ;
#3182 = CARTESIAN_POINT ( 'NONE',  ( 11.00000000000003375, -6.123233995736745575E-16, 20.00000000000003553 ) ) ;
#3183 = EDGE_CURVE ( 'NONE', #8913, #47, #6026, .T. ) ;
#3184 = AXIS2_PLACEMENT_3D ( 'NONE', #246, #8035, #11068 ) ;
#3185 = DIRECTION ( 'NONE',  ( 0.000000000000000000, 0.000000000000000000, 1.000000000000000000 ) ) ;
#3186 = CYLINDRICAL_SURFACE ( 'NONE', #4205, 3.999999999999997335 ) ;
#3187 = DIRECTION ( 'NONE',  ( -1.031682152609352680E-29, -1.000000000000000000, 1.498801083243958569E-15 ) ) ;
#3188 = DIRECTION ( 'NONE',  ( -1.000000000000000000, -0.000000000000000000, -0.000000000000000000 ) ) ;
#3189 = VECTOR ( 'NONE', #7621, 1000.000000000000000 ) ;
#3190 = LINE ( 'NONE', #5169, #6207 ) ;
#3191 = VECTOR ( 'NONE', #4303, 1000.000000000000000 ) ;
#3192 =( LENGTH_UNIT ( ) NAMED_UNIT ( * ) SI_UNIT ( .MILLI., .METRE. ) );
#3193 = ORIENTED_EDGE ( 'NONE', *, *, #3431, .T. ) ;
#3194 = CARTESIAN_POINT ( 'NONE',  ( 19.99999999999999645, -3.055252325922228174, 5.825248672282130613 ) ) ;
#3195 = FACE_BOUND ( 'NONE', #9629, .T. ) ;
#3197 = DIRECTION ( 'NONE',  ( 0.000000000000000000, 1.000000000000000000, 0.000000000000000000 ) ) ;
#3196 = AXIS2_PLACEMENT_3D ( 'NONE', #7099, #11084, #5225 ) ;
#3198 = CARTESIAN_POINT ( 'NONE',  ( -32.85000000000007248, -2.147580246367739864E-29, 1.905105283154350624E-15 ) ) ;
#3199 = ORIENTED_EDGE ( 'NONE', *, *, #5959, .T. ) ;
#3200 = VECTOR ( 'NONE', #11397, 1000.000000000000000 ) ;
#3201 = EDGE_CURVE ( 'NONE', #6863, #2130, #7275, .T. ) ;
#3202 = CARTESIAN_POINT ( 'NONE',  ( 0.000000000000000000, -6.884685972239644514, -2.713134545806132003 ) ) ;
#3203 = EDGE_CURVE ( 'NONE', #9222, #6979, #2103, .T. ) ;
#3204 = ADVANCED_FACE ( 'NONE', ( #12025 ), #8080, .T. ) ;
#3205 = CARTESIAN_POINT ( 'NONE',  ( 40.00000000000000711, 14.39651704831740986, -19.59866274153860388 ) ) ;
#3206 =( NAMED_UNIT ( * ) SI_UNIT ( $, .STERADIAN. ) SOLID_ANGLE_UNIT ( ) );
#3207 = ORIENTED_EDGE ( 'NONE', *, *, #4633, .F. ) ;
#3208 = DIRECTION ( 'NONE',  ( 0.000000000000000000, 0.000000000000000000, 1.000000000000000000 ) ) ;
#3209 = ORIENTED_EDGE ( 'NONE', *, *, #2644, .T. ) ;
#3210 = CIRCLE ( 'NONE', #10372, 6.499000000000009436 ) ;
#3211 = EDGE_LOOP ( 'NONE', ( #2720, #3521, #1959, #7626 ) ) ;
#3212 = SHAPE_DEFINITION_REPRESENTATION ( #12249, #9199 ) ;
#3213 = VECTOR ( 'NONE', #9924, 1000.000000000000000 ) ;
#3214 = CARTESIAN_POINT ( 'NONE',  ( -3.999999999999963585, -2.309401076758515359, -3.433295621305398893 ) ) ;
#3215 = ORIENTED_EDGE ( 'NONE', *, *, #7466, .F. ) ;
#3216 = FACE_OUTER_BOUND ( 'NONE', #11053, .T. ) ;
#3217 = DIRECTION ( 'NONE',  ( 0.000000000000000000, 0.000000000000000000, 1.000000000000000000 ) ) ;
#3218 = ORIENTED_EDGE ( 'NONE', *, *, #3359, .T. ) ;
#3219 = DIRECTION ( 'NONE',  ( 1.000000000000000000, -1.010728034814421376E-30, -1.090846720500930387E-30 ) ) ;
#3220 = CARTESIAN_POINT ( 'NONE',  ( 0.1999999999999987899, 2.343373503925209768E-16, -3.500000000000000000 ) ) ;
#3221 = LINE ( 'NONE', #9941, #7769 ) ;
#3222 = CARTESIAN_POINT ( 'NONE',  ( -1.243802165048778496, 3.900692638707451643, -3.223146290109630829 ) ) ;
#3223 = AXIS2_PLACEMENT_3D ( 'NONE', #1181, #9032, #931 ) ;
#3224 = ADVANCED_FACE ( 'NONE', ( #8145 ), #6149, .T. ) ;
#3225 = CIRCLE ( 'NONE', #10383, 2.149999999999988809 ) ;
#3226 = ORIENTED_EDGE ( 'NONE', *, *, #1999, .F. ) ;
#3227 = EDGE_LOOP ( 'NONE', ( #5568, #775, #11039 ) ) ;
#3228 = ORIENTED_EDGE ( 'NONE', *, *, #5969, .T. ) ;
#3229 = ORIENTED_EDGE ( 'NONE', *, *, #7750, .F. ) ;
#3230 = DIRECTION ( 'NONE',  ( -1.257247067695985463E-30, 0.9749279121818227312, 0.2225209339563182231 ) ) ;
#3231 = ADVANCED_FACE ( 'NONE', ( #7127 ), #8982, .T. ) ;
#3232 = DIRECTION ( 'NONE',  ( -1.848892746611746419E-31, -1.000000000000000000, 3.250006781153460502E-32 ) ) ;
#3233 = ORIENTED_EDGE ( 'NONE', *, *, #12147, .F. ) ;
#3234 = CARTESIAN_POINT ( 'NONE',  ( 19.99999999999999645, 5.895746314278407674, 2.916892913127008935 ) ) ;
#3235 = ORIENTED_EDGE ( 'NONE', *, *, #5502, .F. ) ;
#3236 = DIRECTION ( 'NONE',  ( -1.000000000000000000, 1.010728034814421376E-30, 1.090846720500930387E-30 ) ) ;
#3237 = EDGE_CURVE ( 'NONE', #4592, #7505, #7057, .T. ) ;
#3238 = CARTESIAN_POINT ( 'NONE',  ( 19.99999999999999645, 0.000000000000000000, 0.000000000000000000 ) ) ;
#3239 = ADVANCED_FACE ( 'NONE', ( #10067 ), #1253, .F. ) ;
#3240 = CONICAL_SURFACE ( 'NONE', #12283, 2.059999999999998721, 0.9599310885968738161 ) ;
#3241 = CARTESIAN_POINT ( 'NONE',  ( 20.00000000000000000, 9.597108420813796670, -18.39576936187866352 ) ) ;
#3242 = VERTEX_POINT ( 'NONE', #6339 ) ;
#3243 = DIRECTION ( 'NONE',  ( -1.000000000000000000, 0.000000000000000000, 0.000000000000000000 ) ) ;
#3244 = ORIENTED_EDGE ( 'NONE', *, *, #8545, .T. ) ;
#3245 = DIRECTION ( 'NONE',  ( -1.000000000000000000, 0.000000000000000000, 0.000000000000000000 ) ) ;
#3246 = CARTESIAN_POINT ( 'NONE',  ( -3.999999999999991562, 0.3987449864459988169, -0.01220643443059140493 ) ) ;
#3247 = CIRCLE ( 'NONE', #3042, 6.000000000000000000 ) ;
#3248 = DIRECTION ( 'NONE',  ( 1.848892746611746419E-31, 1.000000000000000000, -3.250006781153460502E-32 ) ) ;
#3249 = CIRCLE ( 'NONE', #8970, 2.800000000000003819 ) ;
#3250 = DIRECTION ( 'NONE',  ( 0.000000000000000000, 5.551115123125776539E-17, 1.000000000000000000 ) ) ;
#3251 = DIRECTION ( 'NONE',  ( -1.154721252774002618E-34, 1.982541115402070533E-16, 1.000000000000000000 ) ) ;
#3252 = FACE_BOUND ( 'NONE', #3650, .T. ) ;
#3253 = PRODUCT_DEFINITION_SHAPE ( 'NONE', 'NONE',  #12754 ) ;
#3254 = CARTESIAN_POINT ( 'NONE',  ( 19.99999999999999645, -6.484265599627176968, 1.105616797298907716 ) ) ;
#3255 = VECTOR ( 'NONE', #5993, 1000.000000000000000 ) ;
#3256 = AXIS2_PLACEMENT_3D ( 'NONE', #1752, #780, #1812 ) ;
#3257 = CARTESIAN_POINT ( 'NONE',  ( 19.99999999999999645, -5.492355906873422455, 4.959236492871922586 ) ) ;
#3258 = EDGE_CURVE ( 'NONE', #9939, #10595, #12628, .T. ) ;
#3259 = EDGE_LOOP ( 'NONE', ( #8750, #11099, #1003, #6879 ) ) ;
#3260 = CARTESIAN_POINT ( 'NONE',  ( 0.000000000000000000, -0.1095571986794155184, -6.498076501567039642 ) ) ;
#3261 = DIRECTION ( 'NONE',  ( 1.000000000000000000, -1.010728034814421376E-30, -1.090846720500930387E-30 ) ) ;
#3262 = DIRECTION ( 'NONE',  ( 1.000000000000000000, 0.000000000000000000, 0.000000000000000000 ) ) ;
#3263 = DIRECTION ( 'NONE',  ( -1.848892746611746419E-31, -1.000000000000000000, 3.250006781153460502E-32 ) ) ;
#3264 = ORIENTED_EDGE ( 'NONE', *, *, #6280, .T. ) ;
#3265 = CIRCLE ( 'NONE', #10433, 9.999999999999998224 ) ;
#3266 = CYLINDRICAL_SURFACE ( 'NONE', #7326, 6.499000000000010324 ) ;
#3267 = CARTESIAN_POINT ( 'NONE',  ( -18.00000000000001421, 29.99999999999999289, 2.000000000000004885 ) ) ;
#3268 = LINE ( 'NONE', #4472, #11092 ) ;
#3269 = ORIENTED_EDGE ( 'NONE', *, *, #10839, .T. ) ;
#3270 = DIRECTION ( 'NONE',  ( 1.000000000000000000, 0.000000000000000000, 0.000000000000000000 ) ) ;
#3271 = EDGE_LOOP ( 'NONE', ( #4453, #8960, #6681, #10701 ) ) ;
#3272 = ORIENTED_EDGE ( 'NONE', *, *, #62, .T. ) ;
#3273 = EDGE_CURVE ( 'NONE', #8777, #9626, #1290, .T. ) ;
#3274 = DIRECTION ( 'NONE',  ( -1.000000000000000000, 1.010728034814421376E-30, 1.090846720500930387E-30 ) ) ;
#3275 = EDGE_CURVE ( 'NONE', #4118, #7374, #262, .T. ) ;
#3276 = ORIENTED_EDGE ( 'NONE', *, *, #8405, .T. ) ;
#3277 = CARTESIAN_POINT ( 'NONE',  ( 15.00000000000003375, 12.50000000000000000, -4.062508476441825628E-31 ) ) ;
#3278 = DIRECTION ( 'NONE',  ( -1.000000000000000000, -1.081682119347366444E-16, 5.551115123125780237E-17 ) ) ;
#3279 = DIRECTION ( 'NONE',  ( 1.000000000000000000, 0.000000000000000000, 0.000000000000000000 ) ) ;
#3280 = CARTESIAN_POINT ( 'NONE',  ( 19.99999999999999645, -2.385831757338583881, 6.045230171438861433 ) ) ;
#3281 = CYLINDRICAL_SURFACE ( 'NONE', #2201, 7.400000000000010125 ) ;
#3282 = CARTESIAN_POINT ( 'NONE',  ( -0.5469614295415836658, 4.303013824935630893, -3.535263753544197751 ) ) ;
#3283 = VECTOR ( 'NONE', #813, 1000.000000000000000 ) ;
#3284 = ORIENTED_EDGE ( 'NONE', *, *, #12203, .T. ) ;
#3285 = ORIENTED_EDGE ( 'NONE', *, *, #11315, .F. ) ;
#3286 = VERTEX_POINT ( 'NONE', #9409 ) ;
#3287 = ORIENTED_EDGE ( 'NONE', *, *, #5466, .T. ) ;
#3288 = LINE ( 'NONE', #9182, #11387 ) ;
#3289 = EDGE_CURVE ( 'NONE', #1611, #10248, #9311, .T. ) ;
#3290 = VECTOR ( 'NONE', #8410, 1000.000000000000000 ) ;
#3291 = CYLINDRICAL_SURFACE ( 'NONE', #8137, 6.000000000000013323 ) ;
#3292 = VERTEX_POINT ( 'NONE', #4608 ) ;
#3293 = CARTESIAN_POINT ( 'NONE',  ( 0.000000000000000000, -6.213893036447800888, -1.903820982021603436 ) ) ;
#3294 = AXIS2_PLACEMENT_3D ( 'NONE', #3785, #2101, #6748 ) ;
#3295 = ORIENTED_EDGE ( 'NONE', *, *, #2076, .T. ) ;
#3296 = CARTESIAN_POINT ( 'NONE',  ( 11.17157287525379772, -12.99999999999999822, -2.828427124746177856 ) ) ;
#3297 = CARTESIAN_POINT ( 'NONE',  ( 20.00000000000000355, 14.50364731389636397, -24.59751492040896892 ) ) ;
#3298 = DIRECTION ( 'NONE',  ( 1.848892746611746419E-31, 1.000000000000000000, -3.250006781153460502E-32 ) ) ;
#3299 = AXIS2_PLACEMENT_3D ( 'NONE', #6383, #1484, #6454 ) ;
#3300 = VECTOR ( 'NONE', #7458, 999.9999999999998863 ) ;
#3301 = AXIS2_PLACEMENT_3D ( 'NONE', #12148, #8197, #7180 ) ;
#3302 = CARTESIAN_POINT ( 'NONE',  ( -40.00000000000000000, 19.99999999999999645, 2.831145448779744488E-15 ) ) ;
#3303 = ORIENTED_EDGE ( 'NONE', *, *, #3425, .F. ) ;
#3304 = CARTESIAN_POINT ( 'NONE',  ( 9.000000000000017764, -12.50000000000000178, 5.000000000000007994 ) ) ;
#3305 = VERTEX_POINT ( 'NONE', #482 ) ;
#3306 = LINE ( 'NONE', #5218, #10534 ) ;
#3307 = SURFACE_SIDE_STYLE ('',( #11146 ) ) ;
#3308 = ADVANCED_FACE ( 'NONE', ( #420 ), #4413, .T. ) ;
#3309 = DIRECTION ( 'NONE',  ( -1.000000000000000000, 1.010728034814421376E-30, 1.090846720500930387E-30 ) ) ;
#3310 = EDGE_CURVE ( 'NONE', #8569, #1400, #4791, .T. ) ;
#3311 = AXIS2_PLACEMENT_3D ( 'NONE', #8940, #4962, #6899 ) ;
#3312 = VECTOR ( 'NONE', #9016, 1000.000000000000000 ) ;
#3313 = CARTESIAN_POINT ( 'NONE',  ( 19.99999999999999645, 1.531833341630123302, 6.396997380212702922 ) ) ;
#3314 = ADVANCED_FACE ( 'NONE', ( #7501 ), #1635, .T. ) ;
#3315 = DIRECTION ( 'NONE',  ( -1.000000000000000000, 1.010728034814421376E-30, 1.090846720500930387E-30 ) ) ;
#3316 = EDGE_CURVE ( 'NONE', #8854, #5073, #4595, .T. ) ;
#3317 = CARTESIAN_POINT ( 'NONE',  ( 19.99999999999997868, 5.362412286431509578, -3.809543717993867595 ) ) ;
#3318 = DIRECTION ( 'NONE',  ( 0.000000000000000000, 1.000000000000000000, 0.000000000000000000 ) ) ;
#3319 = VERTEX_POINT ( 'NONE', #8525 ) ;
#3320 = CARTESIAN_POINT ( 'NONE',  ( -11.83215956619923226, 30.00000000000000000, 2.000000000000000000 ) ) ;
#3321 = VECTOR ( 'NONE', #8467, 1000.000000000000000 ) ;
#3322 = AXIS2_PLACEMENT_3D ( 'NONE', #4459, #3688, #12583 ) ;
#3323 = DIRECTION ( 'NONE',  ( -1.000000000000000000, 1.010728034814421376E-30, 1.090846720500930387E-30 ) ) ;
#3324 = ORIENTED_EDGE ( 'NONE', *, *, #7361, .T. ) ;
#3325 = CYLINDRICAL_SURFACE ( 'NONE', #9503, 6.499000000000010324 ) ;
#3326 = CARTESIAN_POINT ( 'NONE',  ( 9.999999999999998224, 4.177097350749799709, 6.108343287861219828 ) ) ;
#3327 = CARTESIAN_POINT ( 'NONE',  ( -3.999999999999993339, -0.8232339106130704964, -3.430630286862755174 ) ) ;
#3328 = CARTESIAN_POINT ( 'NONE',  ( 0.000000000000000000, 30.00000000000000000, 0.000000000000000000 ) ) ;
#3329 = CARTESIAN_POINT ( 'NONE',  ( 40.00000000000000711, 21.47552320888931021, -7.222675303056226070 ) ) ;
#3330 =( NAMED_UNIT ( * ) SI_UNIT ( $, .STERADIAN. ) SOLID_ANGLE_UNIT ( ) );
#3331 = ORIENTED_EDGE ( 'NONE', *, *, #4464, .T. ) ;
#3332 = DIRECTION ( 'NONE',  ( 0.000000000000000000, 0.000000000000000000, 1.000000000000000000 ) ) ;
#3333 = EDGE_LOOP ( 'NONE', ( #4773, #7781 ) ) ;
#3334 = VERTEX_POINT ( 'NONE', #1509 ) ;
#3335 = ORIENTED_EDGE ( 'NONE', *, *, #8891, .T. ) ;
#3336 = LINE ( 'NONE', #2167, #3090 ) ;
#3337 = CARTESIAN_POINT ( 'NONE',  ( 9.000000000000035527, -19.99999999999999645, 9.850000000000035172 ) ) ;
#3338 = FACE_OUTER_BOUND ( 'NONE', #738, .T. ) ;
#3339 = DIRECTION ( 'NONE',  ( -0.000000000000000000, -1.000000000000000000, -0.000000000000000000 ) ) ;
#3340 = DIRECTION ( 'NONE',  ( -1.159061634649218351E-16, 0.000000000000000000, -1.000000000000000000 ) ) ;
#3341 = ORIENTED_EDGE ( 'NONE', *, *, #10386, .F. ) ;
#3342 = CARTESIAN_POINT ( 'NONE',  ( -3.455068668934444087, 2.624017327439054359, -3.316620875263493584 ) ) ;
#3343 = CIRCLE ( 'NONE', #8039, 2.800000000000003819 ) ;
#3344 = CARTESIAN_POINT ( 'NONE',  ( 20.00000000000000000, 10.63631887905125950, -9.927230231572497843 ) ) ;
#3345 = ORIENTED_EDGE ( 'NONE', *, *, #183, .F. ) ;
#3346 = ORIENTED_EDGE ( 'NONE', *, *, #3043, .T. ) ;
#3347 = ORIENTED_EDGE ( 'NONE', *, *, #4136, .T. ) ;
#3348 = ORIENTED_EDGE ( 'NONE', *, *, #5521, .F. ) ;
#3349 = CIRCLE ( 'NONE', #4145, 7.400000000000009237 ) ;
#3350 = DIRECTION ( 'NONE',  ( 1.000000000000000000, -1.010728034814421376E-30, -1.090846720500930387E-30 ) ) ;
#3351 = CIRCLE ( 'NONE', #1064, 2.800000000000004263 ) ;
#3352 = PRESENTATION_STYLE_ASSIGNMENT (( #6294 ) ) ;
#3353 = ORIENTED_EDGE ( 'NONE', *, *, #12439, .F. ) ;
#3354 = B_SPLINE_CURVE_WITH_KNOTS ( 'NONE', 3,
 ( #4721, #8651, #3698, #1564, #1626, #5500 ),
 .UNSPECIFIED., .F., .F.,
 ( 4, 2, 4 ),
 ( 0.002365888236227993349, 0.003551327329835085415, 0.004736766423442177049 ),
 .UNSPECIFIED. ) ;
#3355 = FACE_OUTER_BOUND ( 'NONE', #3473, .T. ) ;
#3356 = VERTEX_POINT ( 'NONE', #10454 ) ;
#3357 = CARTESIAN_POINT ( 'NONE',  ( -2.449848172108533007, -3.432307619358755169, -3.503702292528917628 ) ) ;
#3358 = DIRECTION ( 'NONE',  ( -1.000000000000000000, 1.010728034814421376E-30, 1.090846720500930387E-30 ) ) ;
#3359 = EDGE_CURVE ( 'NONE', #1141, #12437, #7069, .T. ) ;
#3360 = DIRECTION ( 'NONE',  ( -1.140150527077241873E-30, 0.000000000000000000, 1.000000000000000000 ) ) ;
#3361 = AXIS2_PLACEMENT_3D ( 'NONE', #9072, #12244, #4251 ) ;
#3362 = ADVANCED_FACE ( 'NONE', ( #7378 ), #10319, .F. ) ;
#3363 = PRODUCT_DEFINITION_CONTEXT ( 'detailed design', #10762, 'design' ) ;
#3364 = EDGE_CURVE ( 'NONE', #2371, #3019, #11178, .T. ) ;
#3365 = DIRECTION ( 'NONE',  ( 1.158639454543359513E-30, -0.1785568947986228838, -0.9839295885986322210 ) ) ;
#3366 = VERTEX_POINT ( 'NONE', #3523 ) ;
#3367 = ORIENTED_EDGE ( 'NONE', *, *, #3878, .T. ) ;
#3368 = CARTESIAN_POINT ( 'NONE',  ( 19.99999999999999645, -6.484265599627167198, -1.105616797299011855 ) ) ;
#3369 = EDGE_CURVE ( 'NONE', #12673, #4184, #10547, .T. ) ;
#3370 = AXIS2_PLACEMENT_3D ( 'NONE', #12394, #7486, #2473 ) ;
#3371 = CARTESIAN_POINT ( 'NONE',  ( -3.999999999999991562, 0.9868501483902569760, -0.09357334158578810290 ) ) ;
#3372 = AXIS2_PLACEMENT_3D ( 'NONE', #5912, #4046, #5975 ) ;
#3373 = CARTESIAN_POINT ( 'NONE',  ( 0.000000000000000000, 0.000000000000000000, 0.000000000000000000 ) ) ;
#3374 = CARTESIAN_POINT ( 'NONE',  ( 19.99999999999999645, -5.682309657208357123, 3.313524683561968942 ) ) ;
#3375 = DIRECTION ( 'NONE',  ( -1.000000000000000000, 0.000000000000000000, 0.000000000000000000 ) ) ;
#3376 = CARTESIAN_POINT ( 'NONE',  ( 0.000000000000000000, 30.00000000000000000, -9.999999999999998224 ) ) ;
#3377 = ORIENTED_EDGE ( 'NONE', *, *, #11293, .T. ) ;
#3378 = DIRECTION ( 'NONE',  ( -1.000000000000000000, 1.010728034814421376E-30, 1.090846720500930387E-30 ) ) ;
#3379 = CARTESIAN_POINT ( 'NONE',  ( 10.00000000000000178, 6.057062246029517816, 4.251117141143491374 ) ) ;
#3380 = FILL_AREA_STYLE ('',( #3501 ) ) ;
#3381 = EDGE_CURVE ( 'NONE', #235, #5304, #476, .T. ) ;
#3382 = AXIS2_PLACEMENT_3D ( 'NONE', #533, #4267, #7301 ) ;
#3383 = ORIENTED_EDGE ( 'NONE', *, *, #1559, .T. ) ;
#3384 = CARTESIAN_POINT ( 'NONE',  ( 19.99999999999999645, 0.000000000000000000, 0.000000000000000000 ) ) ;
#3385 = CARTESIAN_POINT ( 'NONE',  ( 19.99999999999997868, 3.565124043461763037, -5.527927226701607744 ) ) ;
#3386 = FACE_OUTER_BOUND ( 'NONE', #9740, .T. ) ;
#3387 = DIRECTION ( 'NONE',  ( 0.000000000000000000, -1.530455820933490821E-32, 1.000000000000000000 ) ) ;
#3388 = DIRECTION ( 'NONE',  ( 1.140150527077241873E-30, 0.000000000000000000, -1.000000000000000000 ) ) ;
#3389 = EDGE_CURVE ( 'NONE', #1188, #4892, #5571, .T. ) ;
#3390 = CARTESIAN_POINT ( 'NONE',  ( 19.99999999999997868, 6.424561140605097087, -0.9808237102696195642 ) ) ;
#3391 = EDGE_CURVE ( 'NONE', #4606, #8354, #2367, .T. ) ;
#3392 = AXIS2_PLACEMENT_3D ( 'NONE', #9589, #6780, #6593 ) ;
#3393 = EDGE_LOOP ( 'NONE', ( #7871, #9625, #11895, #4353 ) ) ;
#3394 = DIRECTION ( 'NONE',  ( -1.000000000000000000, 1.010728034814421376E-30, 1.090846720500930387E-30 ) ) ;
#3395 = ORIENTED_EDGE ( 'NONE', *, *, #7749, .T. ) ;
#3396 = VERTEX_POINT ( 'NONE', #6279 ) ;
#3397 = CONTEXT_DEPENDENT_SHAPE_REPRESENTATION ( #1973, #11542 ) ;
#3398 = ORIENTED_EDGE ( 'NONE', *, *, #10467, .F. ) ;
#3399 = CIRCLE ( 'NONE', #10568, 2.800000000000004263 ) ;
#3400 = DIRECTION ( 'NONE',  ( -1.000000000000000000, -1.031065855027150586E-29, 2.218671295934095703E-30 ) ) ;
#3401 = CARTESIAN_POINT ( 'NONE',  ( -17.00000000000002842, -20.00000000000000000, 12.00000000000003730 ) ) ;
#3402 = CARTESIAN_POINT ( 'NONE',  ( 28.99999999999999645, 3.558819905435939259E-15, 1.610000000000001874 ) ) ;
#3403 = DIRECTION ( 'NONE',  ( 0.000000000000000000, -1.000000000000000000, 0.000000000000000000 ) ) ;
#3404 = PLANE ( 'NONE',  #7342 ) ;
#3405 = ORIENTED_EDGE ( 'NONE', *, *, #507, .F. ) ;
#3406 = DIRECTION ( 'NONE',  ( 3.437775699846481192E-17, 0.2951046417778634967, 0.9554649393887558739 ) ) ;
#3407 = ADVANCED_FACE ( 'NONE', ( #3584 ), #5311, .F. ) ;
#3408 = PLANE ( 'NONE',  #3510 ) ;
#3409 = EDGE_LOOP ( 'NONE', ( #11844, #1968, #3778, #10857 ) ) ;
#3410 = AXIS2_PLACEMENT_3D ( 'NONE', #122, #4048, #6175 ) ;
#3411 = CIRCLE ( 'NONE', #7719, 2.800000000000002487 ) ;
#3412 = VERTEX_POINT ( 'NONE', #12533 ) ;
#3413 = ORIENTED_EDGE ( 'NONE', *, *, #5811, .F. ) ;
#3414 = VERTEX_POINT ( 'NONE', #3767 ) ;
#3415 = DIRECTION ( 'NONE',  ( -1.000000000000000000, -2.206481006425900381E-16, 8.674603474570138454E-17 ) ) ;
#3416 = ADVANCED_FACE ( 'NONE', ( #981 ), #11500, .T. ) ;
#3417 = CARTESIAN_POINT ( 'NONE',  ( 40.00000000000000711, 22.22477142302764008, -7.338293953734282837 ) ) ;
#3418 = ORIENTED_EDGE ( 'NONE', *, *, #11715, .T. ) ;
#3419 = CARTESIAN_POINT ( 'NONE',  ( -30.00000000000000000, -19.99999999999999645, 1.672083814130526039E-15 ) ) ;
#3420 = ORIENTED_EDGE ( 'NONE', *, *, #1683, .F. ) ;
#3421 = AXIS2_PLACEMENT_3D ( 'NONE', #5133, #12748, #1974 ) ;
#3422 = CARTESIAN_POINT ( 'NONE',  ( 9.999999999999998224, 7.164568425986781897, -1.851744925564387856 ) ) ;
#3423 = DIRECTION ( 'NONE',  ( 1.140150527077241873E-30, 0.000000000000000000, -1.000000000000000000 ) ) ;
#3424 = DIRECTION ( 'NONE',  ( 1.503766100577551302E-30, -0.7818314824680222541, -0.6234898018587429203 ) ) ;
#3425 = EDGE_CURVE ( 'NONE', #8686, #1459, #9714, .T. ) ;
#3426 = DIRECTION ( 'NONE',  ( -1.000000000000000000, 1.010728034814421376E-30, 1.090846720500930387E-30 ) ) ;
#3427 = ORIENTED_EDGE ( 'NONE', *, *, #6040, .T. ) ;
#3428 = ORIENTED_EDGE ( 'NONE', *, *, #1999, .T. ) ;
#3429 = CIRCLE ( 'NONE', #11849, 2.800000000000003819 ) ;
#3430 = DIRECTION ( 'NONE',  ( 0.000000000000000000, 0.000000000000000000, 1.000000000000000000 ) ) ;
#3431 = EDGE_CURVE ( 'NONE', #4174, #10853, #4732, .T. ) ;
#3432 = DIRECTION ( 'NONE',  ( -1.000000000000000000, 1.010728034814421376E-30, 1.090846720500930387E-30 ) ) ;
#3433 = EDGE_CURVE ( 'NONE', #5862, #6619, #733, .T. ) ;
#3434 = DIRECTION ( 'NONE',  ( 0.000000000000000000, 0.000000000000000000, 1.000000000000000000 ) ) ;
#3435 = LINE ( 'NONE', #7353, #4862 ) ;
#3436 = VECTOR ( 'NONE', #4384, 1000.000000000000000 ) ;
#3437 = CYLINDRICAL_SURFACE ( 'NONE', #7093, 2.800000000000003819 ) ;
#3438 = LINE ( 'NONE', #6253, #3491 ) ;
#3439 = ORIENTED_EDGE ( 'NONE', *, *, #10966, .T. ) ;
#3440 = DIRECTION ( 'NONE',  ( -0.000000000000000000, -1.000000000000000000, -0.000000000000000000 ) ) ;
#3441 = CARTESIAN_POINT ( 'NONE',  ( 40.00000000000000711, 8.611173066148737121, -18.09125363591105540 ) ) ;
#3442 = CIRCLE ( 'NONE', #550, 2.149999999999992362 ) ;
#3443 = AXIS2_PLACEMENT_3D ( 'NONE', #1702, #1766, #793 ) ;
#3444 = ADVANCED_FACE ( 'NONE', ( #7756 ), #9791, .T. ) ;
#3445 = ORIENTED_EDGE ( 'NONE', *, *, #12352, .T. ) ;
#3446 = DIRECTION ( 'NONE',  ( -1.000000000000000000, -1.031065855027150586E-29, 2.218671295934095703E-30 ) ) ;
#3447 = CARTESIAN_POINT ( 'NONE',  ( 9.999999999999980460, -3.612733913993635859, 6.458185013351679160 ) ) ;
#3448 = LINE ( 'NONE', #6661, #11465 ) ;
#3449 = FACE_OUTER_BOUND ( 'NONE', #301, .T. ) ;
#3450 = FACE_OUTER_BOUND ( 'NONE', #12688, .T. ) ;
#3451 = AXIS2_PLACEMENT_3D ( 'NONE', #2806, #10632, #1753 ) ;
#3452 = CARTESIAN_POINT ( 'NONE',  ( 14.00000000000000000, -30.00000000000000000, 0.000000000000000000 ) ) ;
#3453 = CIRCLE ( 'NONE', #5088, 2.800000000000004263 ) ;
#3454 = DIRECTION ( 'NONE',  ( 1.238279320584846685E-16, -0.9554649393887560960, 0.2951046417778627751 ) ) ;
#3455 = VERTEX_POINT ( 'NONE', #2690 ) ;
#3456 = DIRECTION ( 'NONE',  ( -1.000000000000000000, 1.006188713385347367E-17, 3.844790828812615713E-17 ) ) ;
#3457 = ORIENTED_EDGE ( 'NONE', *, *, #5003, .F. ) ;
#3458 = ORIENTED_EDGE ( 'NONE', *, *, #10519, .T. ) ;
#3459 = ORIENTED_EDGE ( 'NONE', *, *, #3316, .T. ) ;
#3460 = EDGE_CURVE ( 'NONE', #10402, #10850, #922, .T. ) ;
#3461 = ORIENTED_EDGE ( 'NONE', *, *, #10011, .F. ) ;
#3462 = AXIS2_PLACEMENT_3D ( 'NONE', #7581, #11525, #6631 ) ;
#3463 = CARTESIAN_POINT ( 'NONE',  ( 19.99999999999999645, -2.099089055167807860, 6.233932467347772288 ) ) ;
#3464 = ADVANCED_FACE ( 'NONE', ( #3829 ), #6609, .F. ) ;
#3465 = DIRECTION ( 'NONE',  ( -1.000000000000000000, -1.848892746611742259E-31, 1.154721252774410589E-34 ) ) ;
#3466 = FACE_OUTER_BOUND ( 'NONE', #4679, .T. ) ;
#3467 = CARTESIAN_POINT ( 'NONE',  ( 9.999999999999998224, -4.518585619147841292, -5.860237538055118378 ) ) ;
#3468 = EDGE_LOOP ( 'NONE', ( #12230, #6935, #2835, #7511 ) ) ;
#3469 = LINE ( 'NONE', #1454, #11633 ) ;
#3470 = EDGE_CURVE ( 'NONE', #11154, #8658, #8498, .T. ) ;
#3471 = SHAPE_REPRESENTATION ( 'spacer', ( #12422 ), #4543 ) ;
#3472 = CARTESIAN_POINT ( 'NONE',  ( 19.99999999999999645, 0.2110513566293444054, 7.396989747516548697 ) ) ;
#3473 = EDGE_LOOP ( 'NONE', ( #6548, #2562, #665, #424 ) ) ;
#3474 = EDGE_LOOP ( 'NONE', ( #4408, #11578, #2239, #5120 ) ) ;
#3475 = ORIENTED_EDGE ( 'NONE', *, *, #6690, .F. ) ;
#3476 = ORIENTED_EDGE ( 'NONE', *, *, #375, .T. ) ;
#3477 = VERTEX_POINT ( 'NONE', #11624 ) ;
#3478 =( REPRESENTATION_RELATIONSHIP ('NONE','NONE', #10018, #1377 ) REPRESENTATION_RELATIONSHIP_WITH_TRANSFORMATION ( #2363 )SHAPE_REPRESENTATION_RELATIONSHIP( ) );
#3479 = CARTESIAN_POINT ( 'NONE',  ( 28.99999999999999645, 3.469446951953614189E-15, 0.000000000000000000 ) ) ;
#3480 = ORIENTED_EDGE ( 'NONE', *, *, #7586, .T. ) ;
#3481 = FACE_OUTER_BOUND ( 'NONE', #1993, .T. ) ;
#3482 = DIRECTION ( 'NONE',  ( 1.000000000000000000, 1.849040895279789448E-31, -6.938893903907224680E-17 ) ) ;
#3483 = CIRCLE ( 'NONE', #6962, 2.149999999999985256 ) ;
#3484 = CARTESIAN_POINT ( 'NONE',  ( 0.000000000000000000, 0.000000000000000000, 0.000000000000000000 ) ) ;
#3485 = DIRECTION ( 'NONE',  ( 0.000000000000000000, -1.000000000000000000, 0.000000000000000000 ) ) ;
#3486 = ORIENTED_EDGE ( 'NONE', *, *, #10436, .F. ) ;
#3487 = ORIENTED_EDGE ( 'NONE', *, *, #12307, .F. ) ;
#3488 = DIRECTION ( 'NONE',  ( -1.000000000000000000, 0.000000000000000000, 0.000000000000000000 ) ) ;
#3489 = DIRECTION ( 'NONE',  ( 0.000000000000000000, 1.000000000000000000, 0.000000000000000000 ) ) ;
#3490 = CARTESIAN_POINT ( 'NONE',  ( -0.6507732100473482273, 4.243078065514778174, -0.2236248678334831208 ) ) ;
#3491 = VECTOR ( 'NONE', #10160, 1000.000000000000000 ) ;
#3492 = LINE ( 'NONE', #11217, #1995 ) ;
#3493 = CARTESIAN_POINT ( 'NONE',  ( 2.000000000000001776, -1.387778780781445676E-14, -1.535499999999974330 ) ) ;
#3494 = AXIS2_PLACEMENT_3D ( 'NONE', #6432, #2638, #10474 ) ;
#3495 = CARTESIAN_POINT ( 'NONE',  ( 4.000000000000000000, 2.309401076758511806, -0.5000000000000038858 ) ) ;
#3496 = EDGE_CURVE ( 'NONE', #12099, #5977, #24, .T. ) ;
#3497 = EDGE_LOOP ( 'NONE', ( #5062, #11549, #7558, #113 ) ) ;
#3498 = PLANE ( 'NONE',  #205 ) ;
#3499 = CARTESIAN_POINT ( 'NONE',  ( 9.999999999999998224, 2.796709610837451621, -6.851161606081828559 ) ) ;
#3500 = VECTOR ( 'NONE', #11205, 1000.000000000000000 ) ;
#3501 = FILL_AREA_STYLE_COLOUR ( '', #632 ) ;
#3502 = CARTESIAN_POINT ( 'NONE',  ( 0.000000000000000000, 3.681899619563770543, 5.450844343808953774 ) ) ;
#3503 = AXIS2_PLACEMENT_3D ( 'NONE', #3802, #9697, #11659 ) ;
#3504 = ORIENTED_EDGE ( 'NONE', *, *, #8796, .F. ) ;
#3505 = CARTESIAN_POINT ( 'NONE',  ( 19.99999999999997868, 3.565124043461763037, -5.527927226701607744 ) ) ;
#3506 = DIRECTION ( 'NONE',  ( 2.218671295934095002E-30, 5.551115123125776539E-17, 1.000000000000000000 ) ) ;
#3507 = CARTESIAN_POINT ( 'NONE',  ( 0.6448876103708305330, 4.246476118072349593, -0.2256878752776663444 ) ) ;
#3508 = CARTESIAN_POINT ( 'NONE',  ( 14.00000000000000000, 30.00000000000000000, 0.000000000000000000 ) ) ;
#3509 = DIRECTION ( 'NONE',  ( 0.000000000000000000, -1.000000000000000000, 0.000000000000000000 ) ) ;
#3510 = AXIS2_PLACEMENT_3D ( 'NONE', #5318, #12165, #4355 ) ;
#3511 = AXIS2_PLACEMENT_3D ( 'NONE', #4587, #5733, #3627 ) ;
#3512 = AXIS2_PLACEMENT_3D ( 'NONE', #9008, #12247, #7160 ) ;
#3513 = DIRECTION ( 'NONE',  ( -1.000000000000000000, 1.010728034814421376E-30, 1.090846720500930387E-30 ) ) ;
#3514 = EDGE_CURVE ( 'NONE', #5304, #8798, #7631, .T. ) ;
#3515 = EDGE_CURVE ( 'NONE', #12512, #12721, #6407, .T. ) ;
#3516 = CARTESIAN_POINT ( 'NONE',  ( 2.000000000000001776, -0.8865213383406691516, 1.535500000000002085 ) ) ;
#3517 = CYLINDRICAL_SURFACE ( 'NONE', #8257, 24.99999999999999289 ) ;
#3518 = ORIENTED_EDGE ( 'NONE', *, *, #5800, .F. ) ;
#3519 = STYLED_ITEM ( 'NONE', ( #11091 ), #9701 ) ;
#3520 = AXIS2_PLACEMENT_3D ( 'NONE', #11691, #3901, #2699 ) ;
#3521 = ORIENTED_EDGE ( 'NONE', *, *, #8172, .T. ) ;
#3522 = ORIENTED_EDGE ( 'NONE', *, *, #10099, .T. ) ;
#3523 = CARTESIAN_POINT ( 'NONE',  ( 2.000000000000091926, -0.8865213383406727043, -1.535499999999998755 ) ) ;
#3524 = DIRECTION ( 'NONE',  ( -1.000000000000000000, 1.010728034814421376E-30, 1.090846720500930387E-30 ) ) ;
#3525 = CARTESIAN_POINT ( 'NONE',  ( 19.99999999999997868, 5.280167904461786854, -3.922743398397314341 ) ) ;
#3526 = CYLINDRICAL_SURFACE ( 'NONE', #5889, 6.000000000000013323 ) ;
#3527 = VERTEX_POINT ( 'NONE', #7562 ) ;
#3528 = CYLINDRICAL_SURFACE ( 'NONE', #12460, 6.499000000000010324 ) ;
#3529 = FACE_OUTER_BOUND ( 'NONE', #6424, .T. ) ;
#3530 = EDGE_LOOP ( 'NONE', ( #3597, #9990, #8842, #11421 ) ) ;
#3531 = EDGE_CURVE ( 'NONE', #8231, #3178, #3580, .T. ) ;
#3532 = VERTEX_POINT ( 'NONE', #7691 ) ;
#3533 = CARTESIAN_POINT ( 'NONE',  ( 2.000000000000091926, 0.8865213383406691516, -1.535500000000002085 ) ) ;
#3534 = ORIENTED_EDGE ( 'NONE', *, *, #10571, .T. ) ;
#3535 = EDGE_CURVE ( 'NONE', #5702, #9004, #2819, .T. ) ;
#3536 = EDGE_LOOP ( 'NONE', ( #6168, #3218, #12152, #743 ) ) ;
#3537 = ORIENTED_EDGE ( 'NONE', *, *, #4198, .F. ) ;
#3538 = CARTESIAN_POINT ( 'NONE',  ( 0.000000000000000000, 0.000000000000000000, 0.000000000000000000 ) ) ;
#3539 = EDGE_CURVE ( 'NONE', #11717, #12369, #12634, .T. ) ;
#3540 = CARTESIAN_POINT ( 'NONE',  ( 0.000000000000000000, 3.975087478966635945, 6.241688836730221901 ) ) ;
#3541 = CIRCLE ( 'NONE', #1877, 2.149999999999992362 ) ;
#3542 = ORIENTED_EDGE ( 'NONE', *, *, #12091, .T. ) ;
#3543 = DIRECTION ( 'NONE',  ( -1.000000000000000000, 1.010728034814421376E-30, 1.090846720500930387E-30 ) ) ;
#3544 = CARTESIAN_POINT ( 'NONE',  ( 19.99999999999999645, 0.000000000000000000, 0.000000000000000000 ) ) ;
#3545 = CARTESIAN_POINT ( 'NONE',  ( 19.99999999999999645, 0.000000000000000000, 0.000000000000000000 ) ) ;
#3546 = AXIS2_PLACEMENT_3D ( 'NONE', #259, #4191, #8110 ) ;
#3547 = EDGE_CURVE ( 'NONE', #9929, #3010, #9600, .T. ) ;
#3548 = DIRECTION ( 'NONE',  ( 0.000000000000000000, 0.000000000000000000, 1.000000000000000000 ) ) ;
#3549 = EDGE_CURVE ( 'NONE', #5919, #5117, #11684, .T. ) ;
#3550 = EDGE_LOOP ( 'NONE', ( #4460, #8266, #3264, #11637 ) ) ;
#3551 = AXIS2_PLACEMENT_3D ( 'NONE', #10954, #10759, #1038 ) ;
#3552 = ORIENTED_EDGE ( 'NONE', *, *, #7749, .F. ) ;
#3553 =( REPRESENTATION_RELATIONSHIP ('NONE','NONE', #10018, #10094 ) REPRESENTATION_RELATIONSHIP_WITH_TRANSFORMATION ( #10182 )SHAPE_REPRESENTATION_RELATIONSHIP( ) );
#3554 = DIRECTION ( 'NONE',  ( 1.000000000000000000, 5.916456789157575403E-31, -1.224646799147352714E-16 ) ) ;
#3555 = CARTESIAN_POINT ( 'NONE',  ( -4.204015924366180101, 1.626724848190912898, -3.610627190413403742 ) ) ;
#3556 = CARTESIAN_POINT ( 'NONE',  ( 0.000000000000000000, 0.000000000000000000, 0.000000000000000000 ) ) ;
#3557 = CARTESIAN_POINT ( 'NONE',  ( 3.469446951953614189E-14, -3.469446951953614189E-15, -5.000000000000011546 ) ) ;
#3558 = CARTESIAN_POINT ( 'NONE',  ( 2.000000000000001776, -0.8865213383406727043, 1.535500000000009191 ) ) ;
#3559 = ORIENTED_EDGE ( 'NONE', *, *, #5077, .T. ) ;
#3560 = LINE ( 'NONE', #7480, #6164 ) ;
#3561 = CIRCLE ( 'NONE', #3370, 6.499000000000005883 ) ;
#3562 = CARTESIAN_POINT ( 'NONE',  ( 9.000000000000028422, 30.00000000000000000, -9.742497179615118866E-31 ) ) ;
#3563 = EDGE_CURVE ( 'NONE', #2750, #11393, #10703, .T. ) ;
#3564 = AXIS2_PLACEMENT_3D ( 'NONE', #8227, #11128, #6229 ) ;
#3565 = EDGE_CURVE ( 'NONE', #5894, #6626, #12006, .T. ) ;
#3566 = CYLINDRICAL_SURFACE ( 'NONE', #5552, 2.800000000000003819 ) ;
#3567 = ORIENTED_EDGE ( 'NONE', *, *, #7143, .T. ) ;
#3568 = DIRECTION ( 'NONE',  ( -1.000000000000000000, -1.081682119347366197E-16, 6.938893903907228378E-17 ) ) ;
#3569 = CARTESIAN_POINT ( 'NONE',  ( 0.000000000000000000, -5.932103089875909951, -2.654647609586779922 ) ) ;
#3570 = VECTOR ( 'NONE', #4878, 1000.000000000000000 ) ;
#3571 = CARTESIAN_POINT ( 'NONE',  ( 2.000000000000001776, 0.8865213383406622683, -1.535499999999995202 ) ) ;
#3572 = CARTESIAN_POINT ( 'NONE',  ( 0.000000000000000000, 0.000000000000000000, 0.000000000000000000 ) ) ;
#3573 = CARTESIAN_POINT ( 'NONE',  ( 19.99999999999997868, 1.052479792859146723, -6.413211932068299426 ) ) ;
#3574 = VECTOR ( 'NONE', #12296, 1000.000000000000000 ) ;
#3575 = CARTESIAN_POINT ( 'NONE',  ( 9.999999999999998224, 7.380072687735808934, -0.5427035320837159116 ) ) ;
#3576 = FILL_AREA_STYLE_COLOUR ( '', #810 ) ;
#3577 = EDGE_CURVE ( 'NONE', #9099, #11297, #4012, .T. ) ;
#3578 = FACE_BOUND ( 'NONE', #6947, .T. ) ;
#3579 = ORIENTED_EDGE ( 'NONE', *, *, #6176, .F. ) ;
#3580 = CIRCLE ( 'NONE', #10133, 2.800000000000003375 ) ;
#3581 = ORIENTED_EDGE ( 'NONE', *, *, #3997, .F. ) ;
#3582 = ORIENTED_EDGE ( 'NONE', *, *, #10353, .T. ) ;
#3583 = ADVANCED_FACE ( 'NONE', ( #1107 ), #5235, .F. ) ;
#3584 = FACE_OUTER_BOUND ( 'NONE', #11187, .T. ) ;
#3585 = FACE_OUTER_BOUND ( 'NONE', #10006, .T. ) ;
#3587 = EDGE_CURVE ( 'NONE', #7514, #11636, #2135, .T. ) ;
#3586 = DIRECTION ( 'NONE',  ( -1.000000000000000000, 1.010728034814421376E-30, 1.090846720500930387E-30 ) ) ;
#3588 = LINE ( 'NONE', #3467, #12690 ) ;
#3589 = VERTEX_POINT ( 'NONE', #146 ) ;
#3590 = DIRECTION ( 'NONE',  ( -1.000000000000000000, 1.006188713385347367E-17, 3.844790828812615713E-17 ) ) ;
#3591 = AXIS2_PLACEMENT_3D ( 'NONE', #9894, #4780, #6718 ) ;
#3592 = DIRECTION ( 'NONE',  ( 0.000000000000000000, 0.000000000000000000, 1.000000000000000000 ) ) ;
#3593 = ORIENTED_EDGE ( 'NONE', *, *, #7143, .F. ) ;
#3594 = VERTEX_POINT ( 'NONE', #2082 ) ;
#3595 = PLANE ( 'NONE',  #8237 ) ;
#3596 = ORIENTED_EDGE ( 'NONE', *, *, #1243, .F. ) ;
#3597 = ORIENTED_EDGE ( 'NONE', *, *, #12203, .F. ) ;
#3598 = CARTESIAN_POINT ( 'NONE',  ( 4.200000000000001954, 0.000000000000000000, -1.734723475976807094E-14 ) ) ;
#3599 = FILL_AREA_STYLE_COLOUR ( '', #2603 ) ;
#3600 = ORIENTED_EDGE ( 'NONE', *, *, #12188, .T. ) ;
#3601 = DIRECTION ( 'NONE',  ( 0.000000000000000000, -5.551115123125776539E-17, -1.000000000000000000 ) ) ;
#3602 = FACE_BOUND ( 'NONE', #12467, .T. ) ;
#3603 = ORIENTED_EDGE ( 'NONE', *, *, #4448, .T. ) ;
#3604 = EDGE_CURVE ( 'NONE', #3737, #6636, #3064, .T. ) ;
#3605 = DIRECTION ( 'NONE',  ( 0.000000000000000000, 0.000000000000000000, 1.000000000000000000 ) ) ;
#3606 = DIRECTION ( 'NONE',  ( -1.000000000000000000, -1.848892746611742259E-31, 1.154721252774410589E-34 ) ) ;
#3607 = VECTOR ( 'NONE', #4061, 1000.000000000000000 ) ;
#3608 = VECTOR ( 'NONE', #8235, 1000.000000000000000 ) ;
#3609 = DIRECTION ( 'NONE',  ( -3.437775699846489820E-17, -0.2951046417778627751, -0.9554649393887560960 ) ) ;
#3610 = CARTESIAN_POINT ( 'NONE',  ( 2.000000000000001776, 8.523737271559639822E-17, 1.535500000000001863 ) ) ;
#3611 = ADVANCED_FACE ( 'NONE', ( #3128 ), #7077, .F. ) ;
#3612 = ORIENTED_EDGE ( 'NONE', *, *, #2120, .F. ) ;
#3613 = ORIENTED_EDGE ( 'NONE', *, *, #5847, .T. ) ;
#3614 = CARTESIAN_POINT ( 'NONE',  ( 20.00000000000000000, 39.34792583643765340, -17.06347054209567560 ) ) ;
#3615 = AXIS2_PLACEMENT_3D ( 'NONE', #7023, #3173, #10934 ) ;
#3616 = DIRECTION ( 'NONE',  ( 0.000000000000000000, 0.000000000000000000, 1.000000000000000000 ) ) ;
#3617 = ORIENTED_EDGE ( 'NONE', *, *, #7517, .F. ) ;
#3618 = VECTOR ( 'NONE', #7958, 1000.000000000000000 ) ;
#3619 = DIRECTION ( 'NONE',  ( -1.000000000000000000, 1.010728034814421376E-30, 1.090846720500930387E-30 ) ) ;
#3620 = ADVANCED_FACE ( 'NONE', ( #3195, #11942 ), #4204, .T. ) ;
#3621 = DIRECTION ( 'NONE',  ( 0.000000000000000000, 0.5877852522924685852, 0.8090169943749506709 ) ) ;
#3622 = EDGE_CURVE ( 'NONE', #11248, #10850, #2283, .T. ) ;
#3623 = FACE_OUTER_BOUND ( 'NONE', #6081, .T. ) ;
#3624 = CIRCLE ( 'NONE', #6910, 2.000000000000000888 ) ;
#3625 = CARTESIAN_POINT ( 'NONE',  ( 19.99999999999999645, -5.492355906873351401, -4.959236492872019397 ) ) ;
#3626 = ORIENTED_EDGE ( 'NONE', *, *, #5180, .F. ) ;
#3627 = DIRECTION ( 'NONE',  ( 7.241496590895993670E-32, 0.6579387259397136978, -0.7530714660036098573 ) ) ;
#3628 = CARTESIAN_POINT ( 'NONE',  ( -4.154094228333783612, -2.398367420967604247, -3.721909803043274234 ) ) ;
#3629 = CYLINDRICAL_SURFACE ( 'NONE', #9449, 2.800000000000003819 ) ;
#3630 = VERTEX_POINT ( 'NONE', #7932 ) ;
#3631 = DIRECTION ( 'NONE',  ( 0.000000000000000000, 0.000000000000000000, -1.000000000000000000 ) ) ;
#3632 = DIRECTION ( 'NONE',  ( 0.000000000000000000, -0.9909497617679332571, -0.1342332658176667581 ) ) ;
#3633 = DIRECTION ( 'NONE',  ( 0.000000000000000000, 0.000000000000000000, 1.000000000000000000 ) ) ;
#3634 = CARTESIAN_POINT ( 'NONE',  ( -7.321615276582515819E-30, 1.831867990631508193E-16, 3.300000000000003375 ) ) ;
#3635 = DIRECTION ( 'NONE',  ( -1.000000000000000000, -1.081682119347366197E-16, 6.938893903907228378E-17 ) ) ;
#3636 = LINE ( 'NONE', #12523, #3189 ) ;
#3637 = EDGE_CURVE ( 'NONE', #2170, #3527, #8302, .T. ) ;
#3638 = UNCERTAINTY_MEASURE_WITH_UNIT (LENGTH_MEASURE( 1.000000000000000082E-05 ), #10533, 'distance_accuracy_value', 'NONE');
#3639 = VECTOR ( 'NONE', #7323, 999.9999999999998863 ) ;
#3640 = PRESENTATION_LAYER_ASSIGNMENT (  '', '', ( #7344 ) ) ;
#3641 = DIRECTION ( 'NONE',  ( 0.000000000000000000, 5.551115123125777155E-17, 1.000000000000000000 ) ) ;
#3642 = ORIENTED_EDGE ( 'NONE', *, *, #11747, .T. ) ;
#3643 = ORIENTED_EDGE ( 'NONE', *, *, #6490, .F. ) ;
#3644 = EDGE_LOOP ( 'NONE', ( #10651, #8593, #5758, #8809 ) ) ;
#3645 = DIRECTION ( 'NONE',  ( 0.000000000000000000, 0.000000000000000000, 1.000000000000000000 ) ) ;
#3646 = DIRECTION ( 'NONE',  ( 1.238279320584846685E-16, -0.9554649393887560960, 0.2951046417778627751 ) ) ;
#3647 = CARTESIAN_POINT ( 'NONE',  ( 20.00000000000000000, 21.12780530657007461, -5.807015647486883481 ) ) ;
#3648 = CIRCLE ( 'NONE', #11049, 2.800000000000002487 ) ;
#3649 = CARTESIAN_POINT ( 'NONE',  ( 14.00000000000000000, 61.31370849898475228, -3.999999999999997335 ) ) ;
#3650 = EDGE_LOOP ( 'NONE', ( #10523, #4157 ) ) ;
#3651 = CARTESIAN_POINT ( 'NONE',  ( 33.00000000000001421, 39.34792583643766761, -17.06347054209568270 ) ) ;
#3652 = CARTESIAN_POINT ( 'NONE',  ( -10.00000000000000178, 0.000000000000000000, 0.000000000000000000 ) ) ;
#3653 = EDGE_LOOP ( 'NONE', ( #11585, #10453, #10007, #3765, #5718, #6710 ) ) ;
#3654 = EDGE_LOOP ( 'NONE', ( #5185, #7120, #215, #8534 ) ) ;
#3655 = ADVANCED_FACE ( 'NONE', ( #8124 ), #9979, .F. ) ;
#3656 = FACE_BOUND ( 'NONE', #7270, .T. ) ;
#3657 = ORIENTED_EDGE ( 'NONE', *, *, #6412, .T. ) ;
#3658 = AXIS2_PLACEMENT_3D ( 'NONE', #12629, #3616, #2654 ) ;
#3659 = EDGE_CURVE ( 'NONE', #1458, #2782, #3177, .T. ) ;
#3660 = VERTEX_POINT ( 'NONE', #9090 ) ;
#3661 = DIRECTION ( 'NONE',  ( -1.000000000000000000, 1.010728034814421376E-30, 1.090846720500930387E-30 ) ) ;
#3662 = CYLINDRICAL_SURFACE ( 'NONE', #3900, 2.100000000000000089 ) ;
#3663 = EDGE_LOOP ( 'NONE', ( #8523, #2860, #12695, #6763 ) ) ;
#3664 = CARTESIAN_POINT ( 'NONE',  ( -7.888106377466153063, 30.00000000000000000, -1.333333333333333703 ) ) ;
#3665 = LINE ( 'NONE', #10475, #3300 ) ;
#3666 = ORIENTED_EDGE ( 'NONE', *, *, #59, .T. ) ;
#3667 = CARTESIAN_POINT ( 'NONE',  ( 3.469446951953614189E-14, -3.469446951953614189E-15, -4.974600000000009459 ) ) ;
#3668 = CARTESIAN_POINT ( 'NONE',  ( 40.00000000000000711, 32.50906206197875292, -8.925292473609246713 ) ) ;
#3669 = CARTESIAN_POINT ( 'NONE',  ( 2.000000000000001776, -1.773042676681348739, 1.387778780781445676E-14 ) ) ;
#3670 = UNCERTAINTY_MEASURE_WITH_UNIT (LENGTH_MEASURE( 1.000000000000000082E-05 ), #5671, 'distance_accuracy_value', 'NONE');
#3671 = VERTEX_POINT ( 'NONE', #5108 ) ;
#3672 = EDGE_CURVE ( 'NONE', #4167, #10195, #11185, .T. ) ;
#3673 = EDGE_LOOP ( 'NONE', ( #4612, #9882, #9043, #10462 ) ) ;
#3674 = FACE_OUTER_BOUND ( 'NONE', #2060, .T. ) ;
#3675 = CARTESIAN_POINT ( 'NONE',  ( 46.00000000000014921, -2.050770054155458214E-13, -19.99999999999986500 ) ) ;
#3676 = ORIENTED_EDGE ( 'NONE', *, *, #9614, .T. ) ;
#3677 = DIRECTION ( 'NONE',  ( -1.429810390713081971E-30, 0.5877852522924685852, 0.8090169943749506709 ) ) ;
#3678 = CARTESIAN_POINT ( 'NONE',  ( 14.00000000000000000, 12.99999999999999822, 4.000000000000000000 ) ) ;
#3679 = CARTESIAN_POINT ( 'NONE',  ( 19.99999999999999645, 6.057062246029508046, 4.251117141143484268 ) ) ;
#3680 = PLANE ( 'NONE',  #1636 ) ;
#3681 = ORIENTED_EDGE ( 'NONE', *, *, #3369, .T. ) ;
#3682 = AXIS2_PLACEMENT_3D ( 'NONE', #5524, #10339, #3601 ) ;
#3683 = DIRECTION ( 'NONE',  ( 0.000000000000000000, -1.530455820933490821E-32, 1.000000000000000000 ) ) ;
#3684 = ORIENTED_EDGE ( 'NONE', *, *, #10386, .T. ) ;
#3685 = EDGE_CURVE ( 'NONE', #4011, #9943, #11096, .T. ) ;
#3686 = DIRECTION ( 'NONE',  ( 0.000000000000000000, 1.530455820933490821E-32, -1.000000000000000000 ) ) ;
#3687 = ADVANCED_FACE ( 'NONE', ( #1299 ), #7873, .T. ) ;
#3688 = DIRECTION ( 'NONE',  ( -1.000000000000000000, 1.010728034814421376E-30, 1.090846720500930387E-30 ) ) ;
#3689 = CIRCLE ( 'NONE', #10867, 2.200000000000001066 ) ;
#3690 = AXIS2_PLACEMENT_3D ( 'NONE', #12175, #1148, #2251 ) ;
#3691 = CARTESIAN_POINT ( 'NONE',  ( 20.00000000000000000, 9.907988025913237351, -23.58742161290648554 ) ) ;
#3692 = EDGE_CURVE ( 'NONE', #4808, #7388, #6922, .T. ) ;
#3693 = CARTESIAN_POINT ( 'NONE',  ( 0.000000000000000000, 0.000000000000000000, 3.469446951953614189E-15 ) ) ;
#3694 = VECTOR ( 'NONE', #11699, 1000.000000000000000 ) ;
#3695 = CARTESIAN_POINT ( 'NONE',  ( 1.828356344711636217, 3.563200125723174239, 6.226539195266360215E-15 ) ) ;
#3696 = CARTESIAN_POINT ( 'NONE',  ( 0.6937372685066846012, -4.453844082567727902, -3.610536846335899774 ) ) ;
#3697 = LINE ( 'NONE', #656, #1344 ) ;
#3698 = CARTESIAN_POINT ( 'NONE',  ( 2.682243648011664039, 3.070208061305297775, -0.04852650426600636779 ) ) ;
#3699 = CARTESIAN_POINT ( 'NONE',  ( -18.00000000000001421, -30.00000000000001421, 3.000000000000008438 ) ) ;
#3700 = AXIS2_PLACEMENT_3D ( 'NONE', #5101, #7166, #6128 ) ;
#3701 = CIRCLE ( 'NONE', #7800, 7.400000000000011902 ) ;
#3702 = DIRECTION ( 'NONE',  ( 0.000000000000000000, 1.000000000000000000, 0.000000000000000000 ) ) ;
#3703 = ORIENTED_EDGE ( 'NONE', *, *, #5230, .T. ) ;
#3704 = VECTOR ( 'NONE', #11968, 1000.000000000000000 ) ;
#3705 = ORIENTED_EDGE ( 'NONE', *, *, #12507, .F. ) ;
#3706 = VERTEX_POINT ( 'NONE', #9855 ) ;
#3707 = DIRECTION ( 'NONE',  ( -1.000000000000000000, -1.031065855027150586E-29, 2.218671295934095703E-30 ) ) ;
#3708 = AXIS2_PLACEMENT_3D ( 'NONE', #5605, #6583, #10497 ) ;
#3709 = DIRECTION ( 'NONE',  ( 2.218671295934095002E-30, 5.551115123125776539E-17, 1.000000000000000000 ) ) ;
#3710 = FACE_OUTER_BOUND ( 'NONE', #10638, .T. ) ;
#3711 = VECTOR ( 'NONE', #6854, 1000.000000000000000 ) ;
#3712 = CIRCLE ( 'NONE', #10688, 2.800000000000002931 ) ;
#3713 = DIRECTION ( 'NONE',  ( 1.000000000000000000, -1.010728034814421376E-30, -1.090846720500930387E-30 ) ) ;
#3714 = ORIENTED_EDGE ( 'NONE', *, *, #7229, .T. ) ;
#3715 = DIRECTION ( 'NONE',  ( -1.000000000000000000, 1.010728034814421376E-30, 1.090846720500930387E-30 ) ) ;
#3716 = VERTEX_POINT ( 'NONE', #5296 ) ;
#3717 = VERTEX_POINT ( 'NONE', #12263 ) ;
#3718 = DIRECTION ( 'NONE',  ( 1.000000000000000000, 1.081682119347366321E-16, -5.551115123125780237E-17 ) ) ;
#3719 = ORIENTED_EDGE ( 'NONE', *, *, #5293, .F. ) ;
#3720 = AXIS2_PLACEMENT_3D ( 'NONE', #4573, #5401, #2519 ) ;
#3721 = ORIENTED_EDGE ( 'NONE', *, *, #4787, .F. ) ;
#3722 = VECTOR ( 'NONE', #8494, 1000.000000000000114 ) ;
#3723 = ADVANCED_FACE ( 'NONE', ( #1620 ), #5360, .T. ) ;
#3724 = CARTESIAN_POINT ( 'NONE',  ( 19.99999999999999645, 5.483475578891613189, 3.488337222187588793 ) ) ;
#3725 = ORIENTED_EDGE ( 'NONE', *, *, #12034, .F. ) ;
#3726 = CARTESIAN_POINT ( 'NONE',  ( 19.99999999999999645, 5.670261409740655623, 3.175710400084685858 ) ) ;
#3727 = LINE ( 'NONE', #9812, #679 ) ;
#3728 = VERTEX_POINT ( 'NONE', #1560 ) ;
#3729 = DIRECTION ( 'NONE',  ( 0.000000000000000000, 1.530455820933490821E-32, -1.000000000000000000 ) ) ;
#3730 = DIRECTION ( 'NONE',  ( -1.000000000000000000, 1.010728034814421376E-30, 1.090846720500930387E-30 ) ) ;
#3731 = VERTEX_POINT ( 'NONE', #9212 ) ;
#3732 = ORIENTED_EDGE ( 'NONE', *, *, #12515, .F. ) ;
#3733 = ORIENTED_EDGE ( 'NONE', *, *, #7689, .F. ) ;
#3734 = DIRECTION ( 'NONE',  ( 5.916456789157575403E-31, -1.000000000000000000, -1.177425296209239362E-30 ) ) ;
#3735 = AXIS2_PLACEMENT_3D ( 'NONE', #6080, #8068, #11956 ) ;
#3736 = DIRECTION ( 'NONE',  ( 1.000000000000000000, 0.000000000000000000, 0.000000000000000000 ) ) ;
#3737 = VERTEX_POINT ( 'NONE', #12138 ) ;
#3738 = CARTESIAN_POINT ( 'NONE',  ( -32.85000000000006537, -2.029837716746816226E-29, 2.000000000000002220 ) ) ;
#3739 = FACE_OUTER_BOUND ( 'NONE', #10941, .T. ) ;
#3740 = EDGE_CURVE ( 'NONE', #5455, #11575, #8448, .T. ) ;
#3741 = EDGE_CURVE ( 'NONE', #4036, #6829, #1493, .T. ) ;
#3742 = EDGE_CURVE ( 'NONE', #5751, #4277, #6037, .T. ) ;
#3743 = VECTOR ( 'NONE', #6907, 1000.000000000000000 ) ;
#3744 = CARTESIAN_POINT ( 'NONE',  ( 2.725741868436138304, -3.045094352033984375, -3.220599429844055894 ) ) ;
#3745 = VECTOR ( 'NONE', #3762, 1000.000000000000000 ) ;
#3746 = CARTESIAN_POINT ( 'NONE',  ( 19.99999999999997868, -2.401522331692818035, -6.999477872697425163 ) ) ;
#3747 = ORIENTED_EDGE ( 'NONE', *, *, #7999, .T. ) ;
#3748 = CARTESIAN_POINT ( 'NONE',  ( 0.000000000000000000, 0.000000000000000000, 0.000000000000000000 ) ) ;
#3749 = EDGE_CURVE ( 'NONE', #10396, #7062, #9396, .T. ) ;
#3750 = ORIENTED_EDGE ( 'NONE', *, *, #9055, .F. ) ;
#3751 = DIRECTION ( 'NONE',  ( 1.000000000000000000, 1.849040895279789448E-31, -6.938893903907224680E-17 ) ) ;
#3752 = DIRECTION ( 'NONE',  ( -1.000000000000000000, 1.010728034814421376E-30, 1.090846720500930387E-30 ) ) ;
#3753 = CIRCLE ( 'NONE', #8677, 6.000000000000013323 ) ;
#3754 = DIRECTION ( 'NONE',  ( -0.000000000000000000, -1.000000000000000000, -0.000000000000000000 ) ) ;
#3755 = CARTESIAN_POINT ( 'NONE',  ( 19.99999999999997868, 3.681899619563859360, -5.450844343808918246 ) ) ;
#3756 = DIRECTION ( 'NONE',  ( 1.000000000000000000, -6.162975822039154730E-33, -4.563833282352349791E-17 ) ) ;
#3757 = DIRECTION ( 'NONE',  ( -1.000000000000000000, 1.010728034814421376E-30, 1.090846720500930387E-30 ) ) ;
#3758 = CARTESIAN_POINT ( 'NONE',  ( 0.000000000000000000, -30.00000000000000000, 0.000000000000000000 ) ) ;
#3759 = DIRECTION ( 'NONE',  ( -1.000000000000000000, 1.010728034814421376E-30, 1.090846720500930387E-30 ) ) ;
#3760 = CIRCLE ( 'NONE', #4373, 6.499000000000008548 ) ;
#3761 = ADVANCED_FACE ( 'NONE', ( #7366 ), #2347, .T. ) ;
#3762 = DIRECTION ( 'NONE',  ( -1.238279320584846685E-16, 0.9554649393887558739, -0.2951046417778634412 ) ) ;
#3763 = VERTEX_POINT ( 'NONE', #11287 ) ;
#3764 = VERTEX_POINT ( 'NONE', #5494 ) ;
#3765 = ORIENTED_EDGE ( 'NONE', *, *, #12715, .T. ) ;
#3766 = VECTOR ( 'NONE', #8123, 1000.000000000000000 ) ;
#3767 = CARTESIAN_POINT ( 'NONE',  ( 19.99999999999999645, 5.200656487704265807, 5.264330166022984869 ) ) ;
#3768 = AXIS2_PLACEMENT_3D ( 'NONE', #3035, #2974, #2914 ) ;
#3769 = DIRECTION ( 'NONE',  ( 1.000000000000000000, -6.162975822039154730E-33, -4.563833282352349791E-17 ) ) ;
#3770 = ADVANCED_FACE ( 'NONE', ( #10171 ), #2541, .T. ) ;
#3771 = DIRECTION ( 'NONE',  ( 0.000000000000000000, -0.7227948638273979931, 0.6910626489868579858 ) ) ;
#3772 = ORIENTED_EDGE ( 'NONE', *, *, #1394, .T. ) ;
#3773 = EDGE_CURVE ( 'NONE', #6729, #7454, #11229, .T. ) ;
#3774 = DIRECTION ( 'NONE',  ( -1.000000000000000000, 1.010728034814421376E-30, 1.090846720500930387E-30 ) ) ;
#3775 = FACE_OUTER_BOUND ( 'NONE', #12610, .T. ) ;
#3776 = ORIENTED_EDGE ( 'NONE', *, *, #5299, .F. ) ;
#3777 = AXIS2_PLACEMENT_3D ( 'NONE', #165, #3084, #1317 ) ;
#3778 = ORIENTED_EDGE ( 'NONE', *, *, #8477, .T. ) ;
#3779 = CARTESIAN_POINT ( 'NONE',  ( 20.00000000000006750, -8.724036641233686229E-16, -20.00000000000000000 ) ) ;
#3780 = VERTEX_POINT ( 'NONE', #9278 ) ;
#3781 = ORIENTED_EDGE ( 'NONE', *, *, #8551, .F. ) ;
#3782 = FILL_AREA_STYLE_COLOUR ( '', #9870 ) ;
#3783 = FACE_OUTER_BOUND ( 'NONE', #6903, .T. ) ;
#3784 = ORIENTED_EDGE ( 'NONE', *, *, #10381, .T. ) ;
#3785 = CARTESIAN_POINT ( 'NONE',  ( 0.000000000000000000, 0.000000000000000000, 0.000000000000000000 ) ) ;
#3786 = DIRECTION ( 'NONE',  ( 1.000000000000000000, 1.081682119347366321E-16, -5.551115123125780237E-17 ) ) ;
#3787 = VERTEX_POINT ( 'NONE', #12204 ) ;
#3788 = VECTOR ( 'NONE', #8899, 1000.000000000000000 ) ;
#3789 = CARTESIAN_POINT ( 'NONE',  ( 0.000000000000000000, 30.00000000000000000, 0.000000000000000000 ) ) ;
#3790 = LINE ( 'NONE', #3668, #913 ) ;
#3791 = ORIENTED_EDGE ( 'NONE', *, *, #2616, .T. ) ;
#3792 = EDGE_CURVE ( 'NONE', #291, #2575, #9317, .T. ) ;
#3793 = VERTEX_POINT ( 'NONE', #8386 ) ;
#3794 = VERTEX_POINT ( 'NONE', #7243 ) ;
#3795 = DIRECTION ( 'NONE',  ( -2.465190328815656418E-32, 1.177425296209236734E-30, 1.000000000000000000 ) ) ;
#3796 = PRODUCT_DEFINITION_SHAPE ( 'NONE', 'NONE',  #12753 ) ;
#3797 = CARTESIAN_POINT ( 'NONE',  ( 46.00000000000009948, 19.99999999999987566, -12.00000000000006395 ) ) ;
#3798 = ORIENTED_EDGE ( 'NONE', *, *, #112, .F. ) ;
#3799 = DIRECTION ( 'NONE',  ( 1.000000000000000000, 1.081682119347366321E-16, -6.938893903907228378E-17 ) ) ;
#3800 = CIRCLE ( 'NONE', #10394, 2.800000000000002931 ) ;
#3801 = CIRCLE ( 'NONE', #12246, 4.000000000000000000 ) ;
#3802 = CARTESIAN_POINT ( 'NONE',  ( -10.00000000000000178, 0.000000000000000000, 0.000000000000000000 ) ) ;
#3803 = DIRECTION ( 'NONE',  ( -1.000000000000000000, 1.010728034814421376E-30, 1.090846720500930387E-30 ) ) ;
#3804 = CARTESIAN_POINT ( 'NONE',  ( 2.000000000000001776, 1.773042676681338303, 0.000000000000000000 ) ) ;
#3805 = ORIENTED_EDGE ( 'NONE', *, *, #3316, .F. ) ;
#3806 = CARTESIAN_POINT ( 'NONE',  ( -0.1410422978106043723, 4.700232962125088676, -3.687027686973631813 ) ) ;
#3807 = CIRCLE ( 'NONE', #2384, 2.800000000000003375 ) ;
#3808 = ORIENTED_EDGE ( 'NONE', *, *, #1842, .F. ) ;
#3809 = CIRCLE ( 'NONE', #5452, 2.149999999999999023 ) ;
#3810 = CARTESIAN_POINT ( 'NONE',  ( 0.000000000000000000, -4.621065432155110564, 4.569765340993028779 ) ) ;
#3811 = EDGE_CURVE ( 'NONE', #12687, #8054, #7477, .T. ) ;
#3812 = EDGE_CURVE ( 'NONE', #10396, #4592, #9523, .T. ) ;
#3813 = FILL_AREA_STYLE_COLOUR ( '', #5353 ) ;
#3814 = CARTESIAN_POINT ( 'NONE',  ( 19.99999999999999645, 4.192831774278975132, 4.965597920955411304 ) ) ;
#3815 = CIRCLE ( 'NONE', #1956, 6.499000000000006771 ) ;
#3816 = CARTESIAN_POINT ( 'NONE',  ( 21.00000000000003197, 12.50000000000000888, 5.000000000000004441 ) ) ;
#3817 = CARTESIAN_POINT ( 'NONE',  ( 0.000000000000000000, 6.359055127044410227, -1.682410996215903731 ) ) ;
#3818 = CARTESIAN_POINT ( 'NONE',  ( 19.99999999999999645, -3.730839900301562206, 5.321450426182494198 ) ) ;
#3819 = CARTESIAN_POINT ( 'NONE',  ( 14.00000000000000000, 30.00000000000000000, 0.000000000000000000 ) ) ;
#3820 = AXIS2_PLACEMENT_3D ( 'NONE', #9734, #3069, #4017 ) ;
#3821 = FACE_OUTER_BOUND ( 'NONE', #11173, .T. ) ;
#3822 = DIRECTION ( 'NONE',  ( 0.000000000000000000, -1.000000000000000000, 0.000000000000000000 ) ) ;
#3823 = CARTESIAN_POINT ( 'NONE',  ( 11.17157287525379772, 30.00000000000000000, -2.828427124746177856 ) ) ;
#3824 = DIRECTION ( 'NONE',  ( 0.000000000000000000, -0.4999999999999992784, 0.8660254037844389297 ) ) ;
#3825 = ADVANCED_FACE ( 'NONE', ( #6395 ), #5634, .T. ) ;
#3826 = AXIS2_PLACEMENT_3D ( 'NONE', #5560, #5679, #6596 ) ;
#3827 = ORIENTED_EDGE ( 'NONE', *, *, #1370, .F. ) ;
#3828 = ORIENTED_EDGE ( 'NONE', *, *, #8453, .T. ) ;
#3829 = FACE_OUTER_BOUND ( 'NONE', #11908, .T. ) ;
#3830 = CYLINDRICAL_SURFACE ( 'NONE', #10864, 7.400000000000010125 ) ;
#3831 = DIRECTION ( 'NONE',  ( -1.140150527077241873E-30, 0.000000000000000000, 1.000000000000000000 ) ) ;
#3832 = VERTEX_POINT ( 'NONE', #5425 ) ;
#3833 = CARTESIAN_POINT ( 'NONE',  ( 0.1999999999999987899, 0.000000000000000000, -1.734723475976807094E-14 ) ) ;
#3834 = AXIS2_PLACEMENT_3D ( 'NONE', #7565, #10323, #1512 ) ;
#3835 = VECTOR ( 'NONE', #3315, 1000.000000000000000 ) ;
#3836 = VERTEX_POINT ( 'NONE', #2604 ) ;
#3837 = VERTEX_POINT ( 'NONE', #3569 ) ;
#3838 = DIRECTION ( 'NONE',  ( -1.000000000000000000, 1.010728034814421376E-30, 1.090846720500930387E-30 ) ) ;
#3839 = ORIENTED_EDGE ( 'NONE', *, *, #7448, .F. ) ;
#3840 = B_SPLINE_CURVE_WITH_KNOTS ( 'NONE', 3,
 ( #2385, #5331, #2319, #11004, #313, #12177, #6109, #10145 ),
 .UNSPECIFIED., .F., .F.,
 ( 4, 2, 2, 4 ),
 ( 2.465131517029315700E-07, 0.001183067374689838287, 0.001774477805458905951, 0.002365888236227973833 ),
 .UNSPECIFIED. ) ;
#3841 = ORIENTED_EDGE ( 'NONE', *, *, #894, .T. ) ;
#3842 = EDGE_CURVE ( 'NONE', #12369, #7005, #4530, .T. ) ;
#3843 =( NAMED_UNIT ( * ) PLANE_ANGLE_UNIT ( ) SI_UNIT ( $, .RADIAN. ) );
#3844 = EDGE_CURVE ( 'NONE', #8348, #5859, #7487, .T. ) ;
#3845 = DIRECTION ( 'NONE',  ( -1.000000000000000000, 1.010728034814421376E-30, 1.090846720500930387E-30 ) ) ;
#3846 = ORIENTED_EDGE ( 'NONE', *, *, #1942, .F. ) ;
#3847 = CIRCLE ( 'NONE', #7951, 2.800000000000002931 ) ;
#3848 = EDGE_CURVE ( 'NONE', #9454, #7175, #7483, .T. ) ;
#3849 = LINE ( 'NONE', #5001, #7989 ) ;
#3850 = CIRCLE ( 'NONE', #6304, 6.499000000000008548 ) ;
#3851 = DIRECTION ( 'NONE',  ( 0.000000000000000000, 0.000000000000000000, -1.000000000000000000 ) ) ;
#3852 = ORIENTED_EDGE ( 'NONE', *, *, #6020, .F. ) ;
#3853 = CARTESIAN_POINT ( 'NONE',  ( 19.99999999999999645, 0.000000000000000000, 0.000000000000000000 ) ) ;
#3854 = EDGE_CURVE ( 'NONE', #11879, #1901, #7891, .T. ) ;
#3855 = DIRECTION ( 'NONE',  ( 0.000000000000000000, -0.7227948638273979931, 0.6910626489868579858 ) ) ;
#3856 = PRODUCT_DEFINITION_FORMATION_WITH_SPECIFIED_SOURCE ( 'ANY', '', #11216, .NOT_KNOWN. ) ;
#3857 = CIRCLE ( 'NONE', #7350, 2.800000000000002487 ) ;
#3858 = ORIENTED_EDGE ( 'NONE', *, *, #7814, .F. ) ;
#3859 = AXIS2_PLACEMENT_3D ( 'NONE', #1623, #7367, #466 ) ;
#3860 = ORIENTED_EDGE ( 'NONE', *, *, #7163, .T. ) ;
#3861 = VERTEX_POINT ( 'NONE', #8578 ) ;
#3862 = DIRECTION ( 'NONE',  ( 1.503766100577551302E-30, -0.6579387259397027066, -0.7530714660036197383 ) ) ;
#3863 = ORIENTED_EDGE ( 'NONE', *, *, #5075, .T. ) ;
#3864 = CYLINDRICAL_SURFACE ( 'NONE', #5129, 2.800000000000003819 ) ;
#3865 = ORIENTED_EDGE ( 'NONE', *, *, #8891, .F. ) ;
#3866 = LINE ( 'NONE', #1799, #2047 ) ;
#3867 = CIRCLE ( 'NONE', #4056, 6.499000000000010324 ) ;
#3868 = B_SPLINE_CURVE_WITH_KNOTS ( 'NONE', 3,
 ( #4001, #4193, #2271, #6188, #4320 ),
 .UNSPECIFIED., .F., .F.,
 ( 4, 1, 4 ),
 ( 0.000000000000000000, 0.002309401076758505790, 0.004618802153517011580 ),
 .UNSPECIFIED. ) ;
#3869 = CARTESIAN_POINT ( 'NONE',  ( 6.000000000000000000, 49.63999999999998636, -5.000000000000000888 ) ) ;
#3870 = ORIENTED_EDGE ( 'NONE', *, *, #5003, .T. ) ;
#3871 = LINE ( 'NONE', #4899, #416 ) ;
#3872 = EDGE_LOOP ( 'NONE', ( #8759, #6873, #11254, #9704 ) ) ;
#3873 = CARTESIAN_POINT ( 'NONE',  ( 2.000000000000001776, -0.8865213383406691516, 1.535500000000002085 ) ) ;
#3874 = DIRECTION ( 'NONE',  ( -1.000000000000000000, -1.031065855027150586E-29, 2.218671295934095703E-30 ) ) ;
#3875 = DIRECTION ( 'NONE',  ( 0.000000000000000000, 0.000000000000000000, -1.000000000000000000 ) ) ;
#3876 = FACE_OUTER_BOUND ( 'NONE', #10135, .T. ) ;
#3877 = CARTESIAN_POINT ( 'NONE',  ( 19.99999999999999645, 5.670261409740655623, 3.175710400084685858 ) ) ;
#3878 = EDGE_CURVE ( 'NONE', #4885, #10785, #5223, .T. ) ;
#3879 = DIRECTION ( 'NONE',  ( 1.000000000000000000, 0.000000000000000000, 0.000000000000000000 ) ) ;
#3880 = AXIS2_PLACEMENT_3D ( 'NONE', #9858, #1043, #8964 ) ;
#3881 = DIRECTION ( 'NONE',  ( 0.000000000000000000, 1.224646799147353207E-16, 1.000000000000000000 ) ) ;
#3882 = PLANE ( 'NONE',  #8832 ) ;
#3883 = DIRECTION ( 'NONE',  ( -3.437775699846481192E-17, -0.2951046417778634967, -0.9554649393887558739 ) ) ;
#3884 = VECTOR ( 'NONE', #318, 1000.000000000000000 ) ;
#3885 = CIRCLE ( 'NONE', #9832, 6.000000000000000000 ) ;
#3886 = ORIENTED_EDGE ( 'NONE', *, *, #6204, .T. ) ;
#3887 = VERTEX_POINT ( 'NONE', #12646 ) ;
#3888 = DIRECTION ( 'NONE',  ( 0.000000000000000000, -0.1785568947986228838, -0.9839295885986322210 ) ) ;
#3889 =( NAMED_UNIT ( * ) SI_UNIT ( $, .STERADIAN. ) SOLID_ANGLE_UNIT ( ) );
#3890 = DIRECTION ( 'NONE',  ( 0.000000000000000000, 0.000000000000000000, 1.000000000000000000 ) ) ;
#3891 = CARTESIAN_POINT ( 'NONE',  ( 0.000000000000000000, 0.2252065540230630269, -6.573992004634855668 ) ) ;
#3892 = VERTEX_POINT ( 'NONE', #5676 ) ;
#3893 = EDGE_CURVE ( 'NONE', #9064, #8334, #1750, .T. ) ;
#3894 = CARTESIAN_POINT ( 'NONE',  ( 0.000000000000000000, 0.000000000000000000, -0.3080913168122742518 ) ) ;
#3895 = ADVANCED_FACE ( 'NONE', ( #4716 ), #7548, .T. ) ;
#3896 = PRODUCT_RELATED_PRODUCT_CATEGORY ( 'part', '', ( #724 ) ) ;
#3897 = AXIS2_PLACEMENT_3D ( 'NONE', #11809, #5102, #139 ) ;
#3898 = CARTESIAN_POINT ( 'NONE',  ( 3.999999999999999112, -1.221245327087693494E-16, -2.200000000000003730 ) ) ;
#3899 = PRODUCT_DEFINITION_SHAPE ( 'NONE', 'NONE',  #12760 ) ;
#3900 = AXIS2_PLACEMENT_3D ( 'NONE', #4871, #7833, #4684 ) ;
#3901 = DIRECTION ( 'NONE',  ( -1.000000000000000000, 1.010728034814421376E-30, 1.090846720500930387E-30 ) ) ;
#3902 = ORIENTED_EDGE ( 'NONE', *, *, #317, .F. ) ;
#3903 = EDGE_LOOP ( 'NONE', ( #1570, #9581, #1270, #9893 ) ) ;
#3904 = CARTESIAN_POINT ( 'NONE',  ( -45.00000000000001421, 19.99999999999999645, 3.469446951953614189E-15 ) ) ;
#3905 = VERTEX_POINT ( 'NONE', #12585 ) ;
#3906 = VERTEX_POINT ( 'NONE', #9464 ) ;
#3907 = CONICAL_SURFACE ( 'NONE', #8425, 1.535500000000001863, 1.047197551196590748 ) ;
#3908 = CARTESIAN_POINT ( 'NONE',  ( 19.99999999999999645, -6.577476285968334224, 2.730038749995000735 ) ) ;
#3909 = CIRCLE ( 'NONE', #6799, 4.000000000000000000 ) ;
#3910 = EDGE_LOOP ( 'NONE', ( #9964, #4431, #3439, #2166 ) ) ;
#3911 = AXIS2_PLACEMENT_3D ( 'NONE', #5491, #12453, #7612 ) ;
#3912 = DIRECTION ( 'NONE',  ( -1.000000000000000000, 1.010728034814421376E-30, 1.090846720500930387E-30 ) ) ;
#3913 = CARTESIAN_POINT ( 'NONE',  ( 0.000000000000000000, -0.4733669331952392034, 6.481737787550296837 ) ) ;
#3914 = ORIENTED_EDGE ( 'NONE', *, *, #4728, .F. ) ;
#3915 = CARTESIAN_POINT ( 'NONE',  ( 19.99999999999997868, 3.019282868015183752, -6.756029230465944835 ) ) ;
#3916 = CARTESIAN_POINT ( 'NONE',  ( 19.99999999999999645, 4.177097350749791715, 6.108343287861209170 ) ) ;
#3917 = CIRCLE ( 'NONE', #4535, 24.99999999999998934 ) ;
#3918 = ORIENTED_EDGE ( 'NONE', *, *, #4710, .F. ) ;
#3919 = EDGE_LOOP ( 'NONE', ( #5532, #7042, #12541, #10161 ) ) ;
#3920 = ORIENTED_EDGE ( 'NONE', *, *, #11374, .F. ) ;
#3921 = DIRECTION ( 'NONE',  ( -1.000000000000000000, 1.010728034814421376E-30, 1.090846720500930387E-30 ) ) ;
#3922 = ADVANCED_FACE ( 'NONE', ( #121 ), #11673, .F. ) ;
#3923 = VERTEX_POINT ( 'NONE', #4045 ) ;
#3924 = CARTESIAN_POINT ( 'NONE',  ( 4.000000000000000000, -2.309401076758518911, -0.4999999999999917843 ) ) ;
#3925 = ORIENTED_EDGE ( 'NONE', *, *, #9381, .F. ) ;
#3926 = EDGE_CURVE ( 'NONE', #2130, #1272, #10504, .T. ) ;
#3927 = EDGE_CURVE ( 'NONE', #8041, #5416, #2356, .T. ) ;
#3928 = DIRECTION ( 'NONE',  ( -1.000000000000000000, 1.010728034814421376E-30, 1.090846720500930387E-30 ) ) ;
#3929 = DIRECTION ( 'NONE',  ( 0.5000000000000013323, -0.8660254037844379305, 7.395570986446986770E-32 ) ) ;
#3930 = ORIENTED_EDGE ( 'NONE', *, *, #10640, .F. ) ;
#3931 = CARTESIAN_POINT ( 'NONE',  ( 15.00000000000003375, -12.49999999999999645, 3.994800001834461867E-31 ) ) ;
#3932 = ORIENTED_EDGE ( 'NONE', *, *, #8076, .F. ) ;
#3933 = DIRECTION ( 'NONE',  ( -1.000000000000000000, 1.010728034814421376E-30, 1.090846720500930387E-30 ) ) ;
#3934 =( LENGTH_UNIT ( ) NAMED_UNIT ( * ) SI_UNIT ( .MILLI., .METRE. ) );
#3935 = CARTESIAN_POINT ( 'NONE',  ( 20.00000000000006750, -8.724036641233686229E-16, -20.00000000000000000 ) ) ;
#3936 = DIRECTION ( 'NONE',  ( 1.000000000000000000, 1.848892746611742259E-31, -1.154721252774410375E-34 ) ) ;
#3937 = VECTOR ( 'NONE', #4726, 1000.000000000000000 ) ;
#3938 = DIRECTION ( 'NONE',  ( 0.000000000000000000, 0.5128992774059070170, -0.8584487936018656562 ) ) ;
#3939 = DIRECTION ( 'NONE',  ( 0.000000000000000000, 1.000000000000000000, 0.000000000000000000 ) ) ;
#3940 = DIRECTION ( 'NONE',  ( -4.930380657631325535E-31, -1.000000000000000000, -1.177425296209239362E-30 ) ) ;
#3941 = LINE ( 'NONE', #2138, #7192 ) ;
#3942 = EDGE_CURVE ( 'NONE', #8054, #3292, #11608, .T. ) ;
#3943 = CARTESIAN_POINT ( 'NONE',  ( 9.999999999999980460, -4.518585619147922117, 5.860237538055066864 ) ) ;
#3944 = CIRCLE ( 'NONE', #7444, 14.99999999999998934 ) ;
#3945 = DIRECTION ( 'NONE',  ( -0.000000000000000000, -0.000000000000000000, 1.000000000000000000 ) ) ;
#3946 = EDGE_CURVE ( 'NONE', #2242, #2862, #7086, .T. ) ;
#3947 = CIRCLE ( 'NONE', #10935, 10.00000000000000178 ) ;
#3948 = VERTEX_POINT ( 'NONE', #4655 ) ;
#3949 = ORIENTED_EDGE ( 'NONE', *, *, #1801, .T. ) ;
#3950 = DIRECTION ( 'NONE',  ( -1.000000000000000000, 0.000000000000000000, 0.000000000000000000 ) ) ;
#3951 = CARTESIAN_POINT ( 'NONE',  ( 19.99999999999999645, -6.969736844459680114, -2.486517307195224902 ) ) ;
#3952 = PLANE ( 'NONE',  #5930 ) ;
#3953 = DIRECTION ( 'NONE',  ( 0.000000000000000000, 0.000000000000000000, -1.000000000000000000 ) ) ;
#3954 = ORIENTED_EDGE ( 'NONE', *, *, #8130, .T. ) ;
#3955 = CYLINDRICAL_SURFACE ( 'NONE', #5863, 2.800000000000003819 ) ;
#3956 = VECTOR ( 'NONE', #6375, 1000.000000000000000 ) ;
#3957 = EDGE_CURVE ( 'NONE', #11695, #711, #8923, .T. ) ;
#3958 = DIRECTION ( 'NONE',  ( 0.000000000000000000, 0.000000000000000000, -1.000000000000000000 ) ) ;
#3959 = PLANE ( 'NONE',  #9456 ) ;
#3960 = ORIENTED_EDGE ( 'NONE', *, *, #8920, .F. ) ;
#3961 = ORIENTED_EDGE ( 'NONE', *, *, #4062, .T. ) ;
#3962 = CARTESIAN_POINT ( 'NONE',  ( 3.999999999999999112, 3.915468285211833029E-16, 2.200000000000003730 ) ) ;
#3963 = ORIENTED_EDGE ( 'NONE', *, *, #4068, .F. ) ;
#3964 = VERTEX_POINT ( 'NONE', #9525 ) ;
#3965 = APPLICATION_PROTOCOL_DEFINITION ( 'draft international standard', 'automotive_design', 1998, #1067 ) ;
#3966 = CIRCLE ( 'NONE', #11164, 49.99999999999994316 ) ;
#3967 = EDGE_CURVE ( 'NONE', #10658, #11709, #12518, .T. ) ;
#3968 = CARTESIAN_POINT ( 'NONE',  ( 0.000000000000000000, -30.00000000000000000, 0.000000000000000000 ) ) ;
#3969 = EDGE_CURVE ( 'NONE', #3079, #4528, #6047, .T. ) ;
#3970 = EDGE_LOOP ( 'NONE', ( #3272, #127, #9553, #10244 ) ) ;
#3971 = PRESENTATION_STYLE_ASSIGNMENT (( #2029 ) ) ;
#3972 = EDGE_CURVE ( 'NONE', #2328, #363, #2142, .T. ) ;
#3973 = DIRECTION ( 'NONE',  ( -1.000000000000000000, 1.010728034814421376E-30, 1.090846720500930387E-30 ) ) ;
#3974 = ORIENTED_EDGE ( 'NONE', *, *, #3025, .T. ) ;
#3975 = DIRECTION ( 'NONE',  ( 0.000000000000000000, 0.000000000000000000, 1.000000000000000000 ) ) ;
#3976 = DIRECTION ( 'NONE',  ( 0.000000000000000000, 1.530455820933490821E-32, -1.000000000000000000 ) ) ;
#3977 = EDGE_LOOP ( 'NONE', ( #1247, #7856, #8384, #7936 ) ) ;
#3978 = ORIENTED_EDGE ( 'NONE', *, *, #2280, .T. ) ;
#3979 = ORIENTED_EDGE ( 'NONE', *, *, #1551, .F. ) ;
#3980 = CARTESIAN_POINT ( 'NONE',  ( 15.00000000000003375, 12.50000000000000000, -4.062508476441825628E-31 ) ) ;
#3981 = AXIS2_PLACEMENT_3D ( 'NONE', #7110, #1174, #6198 ) ;
#3982 = ADVANCED_FACE ( 'NONE', ( #6659 ), #10564, .T. ) ;
#3983 = ORIENTED_EDGE ( 'NONE', *, *, #1789, .T. ) ;
#3984 = DIRECTION ( 'NONE',  ( -2.465190328815656418E-32, 1.177425296209236734E-30, 1.000000000000000000 ) ) ;
#3985 = VERTEX_POINT ( 'NONE', #5740 ) ;
#3986 = EDGE_CURVE ( 'NONE', #11644, #8701, #8506, .T. ) ;
#3987 = CYLINDRICAL_SURFACE ( 'NONE', #10792, 4.000000000000000000 ) ;
#3988 = AXIS2_PLACEMENT_3D ( 'NONE', #11488, #2123, #7021 ) ;
#3989 = DIRECTION ( 'NONE',  ( 0.000000000000000000, 0.000000000000000000, 1.000000000000000000 ) ) ;
#3990 = ORIENTED_EDGE ( 'NONE', *, *, #2055, .F. ) ;
#3991 = DIRECTION ( 'NONE',  ( 0.000000000000000000, -0.5000000000000011102, -0.8660254037844379305 ) ) ;
#3992 = ORIENTED_EDGE ( 'NONE', *, *, #2480, .F. ) ;
#3993 = DIRECTION ( 'NONE',  ( 0.000000000000000000, -0.9510565162951502005, -0.3090169943749582204 ) ) ;
#3994 = EDGE_CURVE ( 'NONE', #11719, #11828, #10140, .T. ) ;
#3995 = VECTOR ( 'NONE', #10377, 1000.000000000000000 ) ;
#3996 = DIRECTION ( 'NONE',  ( 1.000000000000000000, 1.081682119347366321E-16, -5.551115123125780237E-17 ) ) ;
#3997 = EDGE_CURVE ( 'NONE', #2783, #12687, #1306, .T. ) ;
#3998 = FACE_OUTER_BOUND ( 'NONE', #3977, .T. ) ;
#3999 = PRODUCT_DEFINITION_SHAPE ( 'NONE', 'NONE',  #12765 ) ;
#4000 = CARTESIAN_POINT ( 'NONE',  ( 19.99999999999999645, 0.000000000000000000, 0.000000000000000000 ) ) ;
#4001 = CARTESIAN_POINT ( 'NONE',  ( -3.999999999999963585, -2.309401076758515359, -3.433295621305398893 ) ) ;
#4002 = EDGE_CURVE ( 'NONE', #477, #4490, #10020, .T. ) ;
#4003 = CARTESIAN_POINT ( 'NONE',  ( -3.999999999999994671, 0.000000000000000000, 8.673617379884035472E-15 ) ) ;
#4004 = AXIS2_PLACEMENT_3D ( 'NONE', #9907, #4783, #7805 ) ;
#4005 = AXIS2_PLACEMENT_3D ( 'NONE', #3156, #10855, #5072 ) ;
#4006 = CARTESIAN_POINT ( 'NONE',  ( 0.000000000000000000, 0.6915992404089872370, 6.462096524400245734 ) ) ;
#4007 = CARTESIAN_POINT ( 'NONE',  ( 2.000000000000001776, -0.8865213383406761460, -1.535499999999995202 ) ) ;
#4008 = DIRECTION ( 'NONE',  ( -1.000000000000000000, 6.162975822039154730E-33, 4.563833282352349791E-17 ) ) ;
#4009 = ORIENTED_EDGE ( 'NONE', *, *, #326, .T. ) ;
#4010 = AXIS2_PLACEMENT_3D ( 'NONE', #8594, #12539, #7698 ) ;
#4011 = VERTEX_POINT ( 'NONE', #7083 ) ;
#4012 = LINE ( 'NONE', #9918, #1096 ) ;
#4013 = CARTESIAN_POINT ( 'NONE',  ( 28.99999999999999645, 1.610000000000000320, 2.775557561562891351E-14 ) ) ;
#4014 = DIRECTION ( 'NONE',  ( 1.000000000000000000, 5.916456789157575403E-31, 2.465190328815656418E-32 ) ) ;
#4015 = DIRECTION ( 'NONE',  ( -1.140150527077241873E-30, 0.000000000000000000, 1.000000000000000000 ) ) ;
#4016 = ORIENTED_EDGE ( 'NONE', *, *, #5344, .F. ) ;
#4017 = DIRECTION ( 'NONE',  ( 0.000000000000000000, 5.551115123125776539E-17, 1.000000000000000000 ) ) ;
#4018 = CARTESIAN_POINT ( 'NONE',  ( 9.000000000000035527, -30.00000000000000000, 25.00000000000007105 ) ) ;
#4019 = CARTESIAN_POINT ( 'NONE',  ( 20.00000000000000000, 12.07894703944102766, -21.64141622710139146 ) ) ;
#4020 = VERTEX_POINT ( 'NONE', #3296 ) ;
#4021 = AXIS2_PLACEMENT_3D ( 'NONE', #1242, #4271, #12142 ) ;
#4022 = ORIENTED_EDGE ( 'NONE', *, *, #12303, .T. ) ;
#4023 = CARTESIAN_POINT ( 'NONE',  ( -3.976033822569857420E-13, 4.796734841935179183, -3.721909803043276455 ) ) ;
#4024 = ORIENTED_EDGE ( 'NONE', *, *, #12200, .T. ) ;
#4025 = EDGE_LOOP ( 'NONE', ( #12184, #1777, #12236, #2379 ) ) ;
#4026 = FACE_OUTER_BOUND ( 'NONE', #1105, .T. ) ;
#4027 = ORIENTED_EDGE ( 'NONE', *, *, #10967, .T. ) ;
#4028 = DIRECTION ( 'NONE',  ( 1.140150527077241873E-30, 0.000000000000000000, -1.000000000000000000 ) ) ;
#4029 = DIRECTION ( 'NONE',  ( 1.000000000000000000, 1.081682119347366321E-16, -5.551115123125780237E-17 ) ) ;
#4030 = ORIENTED_EDGE ( 'NONE', *, *, #7363, .T. ) ;
#4031 = PLANE ( 'NONE',  #354 ) ;
#4032 = DIRECTION ( 'NONE',  ( -1.000000000000000000, 1.010728034814421376E-30, 1.090846720500930387E-30 ) ) ;
#4033 = EDGE_CURVE ( 'NONE', #8673, #3906, #3840, .T. ) ;
#4034 = ADVANCED_FACE ( 'NONE', ( #2188 ), #7147, .T. ) ;
#4035 = ORIENTED_EDGE ( 'NONE', *, *, #7970, .T. ) ;
#4036 = VERTEX_POINT ( 'NONE', #9250 ) ;
#4037 = ORIENTED_EDGE ( 'NONE', *, *, #8454, .F. ) ;
#4038 = AXIS2_PLACEMENT_3D ( 'NONE', #11948, #2085, #10900 ) ;
#4039 = LINE ( 'NONE', #3097, #12209 ) ;
#4040 = CIRCLE ( 'NONE', #1360, 2.800000000000003819 ) ;
#4041 = DIRECTION ( 'NONE',  ( 0.000000000000000000, 1.530455820933490821E-32, -1.000000000000000000 ) ) ;
#4042 = ORIENTED_EDGE ( 'NONE', *, *, #11702, .T. ) ;
#4043 = CARTESIAN_POINT ( 'NONE',  ( 8.000000000000000000, -30.00000000000000000, -7.347880794884119736E-16 ) ) ;
#4044 = ORIENTED_EDGE ( 'NONE', *, *, #8938, .T. ) ;
#4045 = CARTESIAN_POINT ( 'NONE',  ( 9.999999999999998224, 30.00000000000000000, -6.123233995736765296E-16 ) ) ;
#4046 = DIRECTION ( 'NONE',  ( -1.000000000000000000, 1.010728034814421376E-30, 1.090846720500930387E-30 ) ) ;
#4047 = VECTOR ( 'NONE', #6397, 1000.000000000000000 ) ;
#4048 = DIRECTION ( 'NONE',  ( -1.000000000000000000, 1.010728034814421376E-30, 1.090846720500930387E-30 ) ) ;
#4049 = EDGE_CURVE ( 'NONE', #4417, #3169, #12232, .T. ) ;
#4050 = PRODUCT_RELATED_PRODUCT_CATEGORY ( 'part', '', ( #2588 ) ) ;
#4051 = CARTESIAN_POINT ( 'NONE',  ( 0.000000000000000000, 3.019282868015180643, -6.756029230465944835 ) ) ;
#4052 = ORIENTED_EDGE ( 'NONE', *, *, #2147, .F. ) ;
#4053 = CARTESIAN_POINT ( 'NONE',  ( 0.000000000000000000, 4.618802153517009401, -1.040834085586084257E-14 ) ) ;
#4054 = ORIENTED_EDGE ( 'NONE', *, *, #10514, .T. ) ;
#4055 = DIRECTION ( 'NONE',  ( -1.140150527077241873E-30, 0.000000000000000000, 1.000000000000000000 ) ) ;
#4056 = AXIS2_PLACEMENT_3D ( 'NONE', #5591, #3543, #4434 ) ;
#4057 = CARTESIAN_POINT ( 'NONE',  ( 2.059999999999998721, 0.000000000000000000, -0.3080913168122742518 ) ) ;
#4058 = CARTESIAN_POINT ( 'NONE',  ( 0.000000000000000000, 0.000000000000000000, 0.000000000000000000 ) ) ;
#4059 = CARTESIAN_POINT ( 'NONE',  ( -4.211140560182210280, 2.431303136016527144, -3.745885042887430405 ) ) ;
#4060 = DIRECTION ( 'NONE',  ( 0.000000000000000000, 0.000000000000000000, 1.000000000000000000 ) ) ;
#4061 = DIRECTION ( 'NONE',  ( 0.000000000000000000, -1.000000000000000000, 8.560894001270036306E-16 ) ) ;
#4062 = EDGE_CURVE ( 'NONE', #11340, #3477, #9122, .T. ) ;
#4063 = DIRECTION ( 'NONE',  ( 1.000000000000000000, 1.849040895279789448E-31, -6.938893903907224680E-17 ) ) ;
#4064 = ADVANCED_FACE ( 'NONE', ( #8098 ), #1207, .T. ) ;
#4065 = DIRECTION ( 'NONE',  ( 0.000000000000000000, -1.000000000000000000, 0.000000000000000000 ) ) ;
#4066 = DIRECTION ( 'NONE',  ( 0.000000000000000000, 1.000000000000000000, 0.000000000000000000 ) ) ;
#4067 = SURFACE_SIDE_STYLE ('',( #8119 ) ) ;
#4068 = EDGE_CURVE ( 'NONE', #4329, #10248, #12014, .T. ) ;
#4069 = ORIENTED_EDGE ( 'NONE', *, *, #6576, .F. ) ;
#4070 = FACE_BOUND ( 'NONE', #9389, .T. ) ;
#4071 = CARTESIAN_POINT ( 'NONE',  ( 4.200000000000001954, 0.000000000000000000, 0.000000000000000000 ) ) ;
#4072 = CARTESIAN_POINT ( 'NONE',  ( 0.000000000000000000, 6.057062246029573771, -4.251117141143404332 ) ) ;
#4073 = CARTESIAN_POINT ( 'NONE',  ( 0.000000000000000000, -5.774092856145694341, -2.982759240804940148 ) ) ;
#4074 = DIRECTION ( 'NONE',  ( 0.000000000000000000, 0.000000000000000000, 1.000000000000000000 ) ) ;
#4075 = EDGE_LOOP ( 'NONE', ( #7755, #12731 ) ) ;
#4076 = FACE_OUTER_BOUND ( 'NONE', #8667, .T. ) ;
#4077 = EDGE_CURVE ( 'NONE', #10909, #12630, #4192, .T. ) ;
#4078 = DIRECTION ( 'NONE',  ( -1.000000000000000000, 1.010728034814421376E-30, 1.090846720500930387E-30 ) ) ;
#4079 = EDGE_CURVE ( 'NONE', #125, #2328, #12237, .T. ) ;
#4080 = ORIENTED_EDGE ( 'NONE', *, *, #2301, .T. ) ;
#4081 = ORIENTED_EDGE ( 'NONE', *, *, #11867, .T. ) ;
#4082 = CARTESIAN_POINT ( 'NONE',  ( -0.6666666666666659635, 4.233901974057234341, -3.300726591567097579 ) ) ;
#4083 = ORIENTED_EDGE ( 'NONE', *, *, #4701, .T. ) ;
#4084 = ORIENTED_EDGE ( 'NONE', *, *, #2477, .T. ) ;
#4085 = PRODUCT_CONTEXT ( 'NONE', #10101, 'mechanical' ) ;
#4086 = DIRECTION ( 'NONE',  ( 0.000000000000000000, 0.000000000000000000, 1.000000000000000000 ) ) ;
#4087 = ORIENTED_EDGE ( 'NONE', *, *, #7899, .F. ) ;
#4088 = CARTESIAN_POINT ( 'NONE',  ( 40.00000000000000711, 20.75061298173632451, -7.028257169185713416 ) ) ;
#4089 = DIRECTION ( 'NONE',  ( 0.000000000000000000, 0.000000000000000000, 1.000000000000000000 ) ) ;
#4090 = ORIENTED_EDGE ( 'NONE', *, *, #7954, .T. ) ;
#4091 = AXIS2_PLACEMENT_3D ( 'NONE', #392, #9145, #5167 ) ;
#4092 = AXIS2_PLACEMENT_3D ( 'NONE', #3234, #7212, #6169 ) ;
#4093 = LINE ( 'NONE', #9574, #9236 ) ;
#4094 = LINE ( 'NONE', #12030, #2426 ) ;
#4095 = CARTESIAN_POINT ( 'NONE',  ( 27.00000000000000355, 39.49790820824818383, -24.06186359251417883 ) ) ;
#4096 =( GEOMETRIC_REPRESENTATION_CONTEXT ( 3 ) GLOBAL_UNCERTAINTY_ASSIGNED_CONTEXT ( ( #662 ) ) GLOBAL_UNIT_ASSIGNED_CONTEXT ( ( #8919, #227, #5192 ) ) REPRESENTATION_CONTEXT ( 'NONE', 'WORKASPACE' ) );
#4097 = ORIENTED_EDGE ( 'NONE', *, *, #9546, .T. ) ;
#4098 = ORIENTED_EDGE ( 'NONE', *, *, #8187, .F. ) ;
#4099 = EDGE_CURVE ( 'NONE', #12171, #8569, #9940, .T. ) ;
#4100 = ORIENTED_EDGE ( 'NONE', *, *, #10552, .T. ) ;
#4101 = AXIS2_PLACEMENT_3D ( 'NONE', #11916, #2192, #3365 ) ;
#4102 = ORIENTED_EDGE ( 'NONE', *, *, #1446, .T. ) ;
#4103 = VECTOR ( 'NONE', #4661, 1000.000000000000114 ) ;
#4104 = CIRCLE ( 'NONE', #5338, 9.999999999999998224 ) ;
#4105 = CARTESIAN_POINT ( 'NONE',  ( 19.99999999999999645, 3.565124043461683101, 5.527927226701645935 ) ) ;
#4106 = EDGE_CURVE ( 'NONE', #6292, #1618, #4404, .T. ) ;
#4107 = DIRECTION ( 'NONE',  ( 6.938893903907224680E-17, -3.250006781153453386E-32, 1.000000000000000000 ) ) ;
#4108 = VECTOR ( 'NONE', #6282, 1000.000000000000114 ) ;
#4109 = EDGE_LOOP ( 'NONE', ( #6272, #6518, #11240, #8208 ) ) ;
#4110 = DIRECTION ( 'NONE',  ( 4.314083075427402290E-32, -0.7227948638273979931, 0.6910626489868579858 ) ) ;
#4111 = EDGE_LOOP ( 'NONE', ( #4293, #3747, #12155, #545 ) ) ;
#4112 = CARTESIAN_POINT ( 'NONE',  ( -1.391697335622786857, -4.043246145443387896, -3.503898532754379680 ) ) ;
#4113 = VECTOR ( 'NONE', #1323, 1000.000000000000114 ) ;
#4114 = AXIS2_PLACEMENT_3D ( 'NONE', #10944, #7286, #11212 ) ;
#4115 = CARTESIAN_POINT ( 'NONE',  ( 19.99999999999999645, 1.531833341630123302, 6.396997380212702922 ) ) ;
#4116 = CARTESIAN_POINT ( 'NONE',  ( 19.99999999999999645, 0.000000000000000000, 0.000000000000000000 ) ) ;
#4117 =( REPRESENTATION_RELATIONSHIP ('NONE','NONE', #10018, #4436 ) REPRESENTATION_RELATIONSHIP_WITH_TRANSFORMATION ( #9104 )SHAPE_REPRESENTATION_RELATIONSHIP( ) );
#4118 = VERTEX_POINT ( 'NONE', #6171 ) ;
#4119 = CARTESIAN_POINT ( 'NONE',  ( 4.101954839143195919, 2.368264730583003352, -3.681130640444369106 ) ) ;
#4120 = ORIENTED_EDGE ( 'NONE', *, *, #8066, .T. ) ;
#4121 = DIRECTION ( 'NONE',  ( -1.000000000000000000, 1.010728034814421376E-30, 1.090846720500930387E-30 ) ) ;
#4122 = STYLED_ITEM ( 'NONE', ( #5487 ), #2668 ) ;
#4123 = FILL_AREA_STYLE ('',( #2987 ) ) ;
#4124 = ADVANCED_FACE ( 'NONE', ( #1337 ), #5211, .T. ) ;
#4125 = CARTESIAN_POINT ( 'NONE',  ( 19.99999999999999645, -1.113123845672405965, 7.315801754025019754 ) ) ;
#4126 = EDGE_CURVE ( 'NONE', #10385, #8996, #6466, .T. ) ;
#4127 = EDGE_CURVE ( 'NONE', #2832, #8684, #4814, .T. ) ;
#4128 = FACE_OUTER_BOUND ( 'NONE', #11878, .T. ) ;
#4129 = CARTESIAN_POINT ( 'NONE',  ( -2.344047193898590287, -3.265465875126468021, -6.784733907506943744E-16 ) ) ;
#4130 = CARTESIAN_POINT ( 'NONE',  ( 40.00000000000000711, 16.59466514679920479, -6.965300083364795114 ) ) ;
#4131 = DIRECTION ( 'NONE',  ( -1.000000000000000000, 1.010728034814421376E-30, 1.090846720500930387E-30 ) ) ;
#4132 = DIRECTION ( 'NONE',  ( -1.848892746611742259E-31, 1.000000000000000000, -3.250006781153460502E-32 ) ) ;
#4133 = CARTESIAN_POINT ( 'NONE',  ( 40.00000000000000000, 39.34792583643766051, -17.06347054209567915 ) ) ;
#4134 = FILL_AREA_STYLE ('',( #7708 ) ) ;
#4135 = VECTOR ( 'NONE', #3824, 1000.000000000000227 ) ;
#4136 = EDGE_CURVE ( 'NONE', #4592, #6148, #9562, .T. ) ;
#4137 = ORIENTED_EDGE ( 'NONE', *, *, #1660, .T. ) ;
#4138 = CARTESIAN_POINT ( 'NONE',  ( 19.99999999999999645, 0.000000000000000000, 0.000000000000000000 ) ) ;
#4139 = DIRECTION ( 'NONE',  ( -1.000000000000000000, 0.000000000000000000, 0.000000000000000000 ) ) ;
#4140 = DIRECTION ( 'NONE',  ( -1.000000000000000000, 1.010728034814421376E-30, 1.090846720500930387E-30 ) ) ;
#4141 = CARTESIAN_POINT ( 'NONE',  ( -18.00000000000000355, 29.99999999999998224, 3.000000000000008438 ) ) ;
#4142 = CYLINDRICAL_SURFACE ( 'NONE', #4038, 6.499000000000010324 ) ;
#4143 = EDGE_LOOP ( 'NONE', ( #1120, #9739, #12659, #12338, #2381, #6160, #6958, #10639, #3567, #12272, #8998, #8819, #9422, #4803, #7145, #7439 ) ) ;
#4144 = DIRECTION ( 'NONE',  ( 0.000000000000000000, 0.000000000000000000, 1.000000000000000000 ) ) ;
#4145 = AXIS2_PLACEMENT_3D ( 'NONE', #6967, #10882, #1161 ) ;
#4146 = DIRECTION ( 'NONE',  ( -1.000000000000000000, 1.010728034814421376E-30, 1.090846720500930387E-30 ) ) ;
#4147 = EDGE_CURVE ( 'NONE', #3717, #8468, #1530, .T. ) ;
#4148 = VECTOR ( 'NONE', #2341, 1000.000000000000000 ) ;
#4149 = DIRECTION ( 'NONE',  ( 0.000000000000000000, 0.000000000000000000, 1.000000000000000000 ) ) ;
#4150 = ORIENTED_EDGE ( 'NONE', *, *, #12198, .T. ) ;
#4151 = EDGE_CURVE ( 'NONE', #11776, #1400, #10277, .T. ) ;
#4152 = CARTESIAN_POINT ( 'NONE',  ( 0.000000000000000000, -3.469446951953614189E-14, -25.03750572909320837 ) ) ;
#4153 = ORIENTED_EDGE ( 'NONE', *, *, #11715, .F. ) ;
#4154 = EDGE_LOOP ( 'NONE', ( #10074, #7337, #9554, #8349 ) ) ;
#4155 = APPLICATION_PROTOCOL_DEFINITION ( 'draft international standard', 'automotive_design', 1998, #1307 ) ;
#4156 = CARTESIAN_POINT ( 'NONE',  ( 33.00000000000001421, 70.57443853988016258, -5.364737079370081041 ) ) ;
#4157 = ORIENTED_EDGE ( 'NONE', *, *, #1103, .F. ) ;
#4158 = ADVANCED_FACE ( 'NONE', ( #5464 ), #9371, .T. ) ;
#4159 = CYLINDRICAL_SURFACE ( 'NONE', #11300, 6.000000000000000000 ) ;
#4160 = CARTESIAN_POINT ( 'NONE',  ( 40.00000000000000000, 39.34792583643766051, -19.21347054209566707 ) ) ;
#4161 = AXIS2_PLACEMENT_3D ( 'NONE', #8042, #5922, #11731 ) ;
#4162 = VERTEX_POINT ( 'NONE', #12493 ) ;
#4163 = CARTESIAN_POINT ( 'NONE',  ( 20.00000000000000000, 39.34792583643766051, -17.06347054209567915 ) ) ;
#4164 = DIRECTION ( 'NONE',  ( 0.000000000000000000, 1.000000000000000000, 0.000000000000000000 ) ) ;
#4165 = DIRECTION ( 'NONE',  ( 0.000000000000000000, 0.000000000000000000, 1.000000000000000000 ) ) ;
#4166 = EDGE_LOOP ( 'NONE', ( #7838, #12636, #10334, #6623 ) ) ;
#4167 = VERTEX_POINT ( 'NONE', #569 ) ;
#4168 = VECTOR ( 'NONE', #10503, 1000.000000000000000 ) ;
#4169 = VERTEX_POINT ( 'NONE', #9500 ) ;
#4170 = VECTOR ( 'NONE', #7207, 1000.000000000000000 ) ;
#4171 = ORIENTED_EDGE ( 'NONE', *, *, #3994, .T. ) ;
#4172 = CARTESIAN_POINT ( 'NONE',  ( 33.00000000000001421, 39.34792583643766761, -19.56347054209567204 ) ) ;
#4173 = FACE_BOUND ( 'NONE', #8027, .T. ) ;
#4174 = VERTEX_POINT ( 'NONE', #9433 ) ;
#4175 = DIRECTION ( 'NONE',  ( -1.000000000000000000, 1.010728034814421376E-30, 1.090846720500930387E-30 ) ) ;
#4176 = VERTEX_POINT ( 'NONE', #1467 ) ;
#4177 = AXIS2_PLACEMENT_3D ( 'NONE', #6089, #4029, #8921 ) ;
#4178 = DIRECTION ( 'NONE',  ( 1.000000000000000000, 1.849040895279789448E-31, -6.938893903907224680E-17 ) ) ;
#4179 = AXIS2_PLACEMENT_3D ( 'NONE', #9968, #1094, #11992 ) ;
#4180 = VECTOR ( 'NONE', #6624, 1000.000000000000114 ) ;
#4181 = EDGE_CURVE ( 'NONE', #3319, #753, #3867, .T. ) ;
#4182 = DIRECTION ( 'NONE',  ( -1.000000000000000000, 1.010728034814421376E-30, 1.090846720500930387E-30 ) ) ;
#4183 = DIRECTION ( 'NONE',  ( 1.000000000000000000, -1.010728034814421376E-30, -1.090846720500930387E-30 ) ) ;
#4184 = VERTEX_POINT ( 'NONE', #2715 ) ;
#4185 = CARTESIAN_POINT ( 'NONE',  ( 14.00000000000000000, 13.00000000000000000, 0.000000000000000000 ) ) ;
#4186 = AXIS2_PLACEMENT_3D ( 'NONE', #4071, #7992, #10047 ) ;
#4187 = VERTEX_POINT ( 'NONE', #7460 ) ;
#4188 = DIRECTION ( 'NONE',  ( -1.000000000000000000, 1.010728034814421376E-30, 1.090846720500930387E-30 ) ) ;
#4189 =( NAMED_UNIT ( * ) PLANE_ANGLE_UNIT ( ) SI_UNIT ( $, .RADIAN. ) );
#4190 = LINE ( 'NONE', #1220, #9860 ) ;
#4191 = DIRECTION ( 'NONE',  ( -4.930380657631325535E-31, -1.000000000000000000, -1.177425296209239362E-30 ) ) ;
#4192 = CIRCLE ( 'NONE', #12644, 2.800000000000003375 ) ;
#4193 = CARTESIAN_POINT ( 'NONE',  ( -3.333333333333297954, -2.694301256218267326, -3.300726591567099355 ) ) ;
#4194 = PLANE ( 'NONE',  #8520 ) ;
#4195 = FACE_OUTER_BOUND ( 'NONE', #9420, .T. ) ;
#4196 = ADVANCED_FACE ( 'NONE', ( #691 ), #2220, .F. ) ;
#4197 = CARTESIAN_POINT ( 'NONE',  ( -31.74999999999995026, 1.339070573669553325E-16, -1.999999999999996225 ) ) ;
#4198 = EDGE_CURVE ( 'NONE', #1661, #9551, #10408, .T. ) ;
#4199 = AXIS2_PLACEMENT_3D ( 'NONE', #5619, #2608, #9532 ) ;
#4200 = CARTESIAN_POINT ( 'NONE',  ( 33.00000000000001421, 39.34792583643766761, -17.06347054209568270 ) ) ;
#4201 = CIRCLE ( 'NONE', #12027, 6.999999999999999112 ) ;
#4202 = ORIENTED_EDGE ( 'NONE', *, *, #8917, .T. ) ;
#4203 = CARTESIAN_POINT ( 'NONE',  ( 19.99999999999997868, -7.258495115966569600, -1.440225208600917739 ) ) ;
#4204 = PLANE ( 'NONE',  #7882 ) ;
#4206 = CARTESIAN_POINT ( 'NONE',  ( 19.99999999999999645, 7.380072687735814263, 0.5427035320837090282 ) ) ;
#4205 = AXIS2_PLACEMENT_3D ( 'NONE', #9971, #11021, #9081 ) ;
#4207 = CARTESIAN_POINT ( 'NONE',  ( 19.99999999999999645, -6.577476285968334224, -0.06996125000500313940 ) ) ;
#4208 = ORIENTED_EDGE ( 'NONE', *, *, #3054, .F. ) ;
#4209 = CONICAL_SURFACE ( 'NONE', #12450, 4.000000000000000000, 0.8911886515913786111 ) ;
#4210 = DIRECTION ( 'NONE',  ( 1.031065855027150586E-29, -1.000000000000000000, 5.551115123125776539E-17 ) ) ;
#4211 = DIRECTION ( 'NONE',  ( -1.000000000000000000, 1.010728034814421376E-30, 1.090846720500930387E-30 ) ) ;
#4212 = FACE_OUTER_BOUND ( 'NONE', #4560, .T. ) ;
#4213 = ORIENTED_EDGE ( 'NONE', *, *, #7256, .T. ) ;
#4214 = DIRECTION ( 'NONE',  ( 0.000000000000000000, 0.000000000000000000, -1.000000000000000000 ) ) ;
#4215 = ORIENTED_EDGE ( 'NONE', *, *, #5869, .F. ) ;
#4216 = AXIS2_PLACEMENT_3D ( 'NONE', #63, #958, #2980 ) ;
#4217 = ORIENTED_EDGE ( 'NONE', *, *, #4079, .F. ) ;
#4218 = CONTEXT_DEPENDENT_SHAPE_REPRESENTATION ( #10274, #1116 ) ;
#4219 = CARTESIAN_POINT ( 'NONE',  ( 0.000000000000000000, -6.413745496774080124, -3.691052519622338490 ) ) ;
#4220 = ORIENTED_EDGE ( 'NONE', *, *, #10680, .F. ) ;
#4221 = DIRECTION ( 'NONE',  ( 0.000000000000000000, 0.000000000000000000, 1.000000000000000000 ) ) ;
#4222 = DIRECTION ( 'NONE',  ( 1.140150527077241873E-30, 0.000000000000000000, -1.000000000000000000 ) ) ;
#4223 = ORIENTED_EDGE ( 'NONE', *, *, #4455, .T. ) ;
#4224 = DIRECTION ( 'NONE',  ( 0.000000000000000000, 1.000000000000000000, 0.000000000000000000 ) ) ;
#4225 = CARTESIAN_POINT ( 'NONE',  ( 4.200000000000001954, 1.339070573674521670E-16, -2.000000000000000888 ) ) ;
#4226 = LINE ( 'NONE', #5314, #11246 ) ;
#4227 = LINE ( 'NONE', #8151, #9755 ) ;
#4228 = CIRCLE ( 'NONE', #4021, 4.000000000000000000 ) ;
#4229 = EDGE_LOOP ( 'NONE', ( #7376, #3461, #1024, #10894 ) ) ;
#4230 = EDGE_CURVE ( 'NONE', #8468, #6636, #6948, .T. ) ;
#4231 = ORIENTED_EDGE ( 'NONE', *, *, #1553, .T. ) ;
#4232 = ORIENTED_EDGE ( 'NONE', *, *, #8987, .F. ) ;
#4233 = ADVANCED_FACE ( 'NONE', ( #4569 ), #8480, .T. ) ;
#4234 = ORIENTED_EDGE ( 'NONE', *, *, #1356, .F. ) ;
#4235 = CARTESIAN_POINT ( 'NONE',  ( 11.17157287525379772, -30.00000000000000000, -2.828427124746177856 ) ) ;
#4236 = CARTESIAN_POINT ( 'NONE',  ( 9.000000000000028422, -30.00000000000000000, 1.387778780781457755E-16 ) ) ;
#4237 = EDGE_LOOP ( 'NONE', ( #3504, #10227, #11106, #1111, #4887, #11159, #5172, #4346, #12022, #1652, #5776, #7252, #6142, #50, #7426, #10177 ) ) ;
#4238 = AXIS2_PLACEMENT_3D ( 'NONE', #1416, #10035, #8114 ) ;
#4239 = EDGE_CURVE ( 'NONE', #10242, #2523, #9974, .T. ) ;
#4240 = STYLED_ITEM ( 'NONE', ( #3352 ), #5724 ) ;
#4241 = CARTESIAN_POINT ( 'NONE',  ( 19.99999999999999645, -6.459281472512945932, 1.243290685169349485 ) ) ;
#4242 = ORIENTED_EDGE ( 'NONE', *, *, #2568, .F. ) ;
#4243 = DIRECTION ( 'NONE',  ( -1.000000000000000000, 1.010728034814421376E-30, 1.090846720500930387E-30 ) ) ;
#4244 = CARTESIAN_POINT ( 'NONE',  ( 0.000000000000000000, 0.000000000000000000, 0.000000000000000000 ) ) ;
#4245 = AXIS2_PLACEMENT_3D ( 'NONE', #7822, #2822, #984 ) ;
#4246 = CARTESIAN_POINT ( 'NONE',  ( 14.00000000000000000, -30.00000000000000000, 0.000000000000000000 ) ) ;
#4247 = TOROIDAL_SURFACE ( 'NONE', #6726, 3.299999999999999822, 0.2000000000000000111 ) ;
#4248 = ORIENTED_EDGE ( 'NONE', *, *, #1608, .F. ) ;
#4249 = DIRECTION ( 'NONE',  ( 0.000000000000000000, 1.000000000000000000, 0.000000000000000000 ) ) ;
#4250 = VERTEX_POINT ( 'NONE', #1662 ) ;
#4251 = DIRECTION ( 'NONE',  ( 0.000000000000000000, 0.000000000000000000, 1.000000000000000000 ) ) ;
#4252 = FACE_OUTER_BOUND ( 'NONE', #4143, .T. ) ;
#4253 = AXIS2_PLACEMENT_3D ( 'NONE', #3067, #12008, #11032 ) ;
#4254 = CARTESIAN_POINT ( 'NONE',  ( 15.00000000000003375, -12.49999999999999645, 4.000000000000000000 ) ) ;
#4255 = AXIS2_PLACEMENT_3D ( 'NONE', #982, #11815, #9857 ) ;
#4256 = DIRECTION ( 'NONE',  ( -1.000000000000000000, 1.010728034814421376E-30, 1.090846720500930387E-30 ) ) ;
#4257 = DIRECTION ( 'NONE',  ( 0.000000000000000000, 0.000000000000000000, -1.000000000000000000 ) ) ;
#4258 = CARTESIAN_POINT ( 'NONE',  ( 19.99999999999999645, 0.000000000000000000, 0.000000000000000000 ) ) ;
#4259 = AXIS2_PLACEMENT_3D ( 'NONE', #6510, #11655, #7531 ) ;
#4260 = DIRECTION ( 'NONE',  ( -1.000000000000000000, -1.031065855027150586E-29, 2.218671295934095703E-30 ) ) ;
#4261 = AXIS2_PLACEMENT_3D ( 'NONE', #260, #7098, #3185 ) ;
#4262 = AXIS2_PLACEMENT_3D ( 'NONE', #5297, #9980, #7244 ) ;
#4263 = DIRECTION ( 'NONE',  ( -1.000000000000000000, 1.006188713385347367E-17, 3.844790828812615713E-17 ) ) ;
#4264 = ORIENTED_EDGE ( 'NONE', *, *, #8206, .T. ) ;
#4265 = CARTESIAN_POINT ( 'NONE',  ( 40.00000000000000711, 11.45997319858345342, -23.64547756539571566 ) ) ;
#4266 = ADVANCED_FACE ( 'NONE', ( #4627 ), #8547, .F. ) ;
#4267 = DIRECTION ( 'NONE',  ( -1.000000000000000000, 1.010728034814421376E-30, 1.090846720500930387E-30 ) ) ;
#4268 = DIRECTION ( 'NONE',  ( -1.000000000000000000, 1.010728034814421376E-30, 1.090846720500930387E-30 ) ) ;
#4269 = LINE ( 'NONE', #8194, #562 ) ;
#4270 = VECTOR ( 'NONE', #6881, 1000.000000000000000 ) ;
#4271 = DIRECTION ( 'NONE',  ( 0.000000000000000000, 1.000000000000000000, 0.000000000000000000 ) ) ;
#4272 = CARTESIAN_POINT ( 'NONE',  ( -4.000000000000001776, 2.309401076758498039, -0.4999999999999935052 ) ) ;
#4273 = CARTESIAN_POINT ( 'NONE',  ( 19.99999999999999645, -6.213893036447818652, 1.903820982021499297 ) ) ;
#4274 = ORIENTED_EDGE ( 'NONE', *, *, #9811, .F. ) ;
#4275 = LINE ( 'NONE', #2360, #9888 ) ;
#4276 = VERTEX_POINT ( 'NONE', #10540 ) ;
#4277 = VERTEX_POINT ( 'NONE', #1725 ) ;
#4278 = ITEM_DEFINED_TRANSFORMATION ( 'NONE', 'NONE', #6534,  #12422 ) ;
#4279 = VERTEX_POINT ( 'NONE', #755 ) ;
#4280 = DIRECTION ( 'NONE',  ( -1.000000000000000000, 1.010728034814421376E-30, 1.090846720500930387E-30 ) ) ;
#4281 = ADVANCED_FACE ( 'NONE', ( #3481 ), #4690, .F. ) ;
#4282 = DIRECTION ( 'NONE',  ( -1.000000000000000000, -5.916456789157575403E-31, 1.577021341797099039E-16 ) ) ;
#4283 = EDGE_CURVE ( 'NONE', #9287, #5879, #2446, .T. ) ;
#4284 = DIRECTION ( 'NONE',  ( 1.000000000000000000, -1.010728034814421376E-30, -1.090846720500930387E-30 ) ) ;
#4286 = ADVANCED_FACE ( 'NONE', ( #8741 ), #5095, .T. ) ;
#4285 = LINE ( 'NONE', #1256, #4699 ) ;
#4287 = CARTESIAN_POINT ( 'NONE',  ( 19.99999999999999645, -4.046291478462170410, -5.186098161460359179 ) ) ;
#4288 = CARTESIAN_POINT ( 'NONE',  ( -2.725741868436132531, 3.045094352033964835, -3.220599429844243300 ) ) ;
#4289 = VECTOR ( 'NONE', #5943, 1000.000000000000000 ) ;
#4290 = DIRECTION ( 'NONE',  ( -1.000000000000000000, 1.010728034814421376E-30, 1.090846720500930387E-30 ) ) ;
#4291 = VERTEX_POINT ( 'NONE', #4815 ) ;
#4292 = VERTEX_POINT ( 'NONE', #10660 ) ;
#4293 = ORIENTED_EDGE ( 'NONE', *, *, #5727, .T. ) ;
#4294 = ORIENTED_EDGE ( 'NONE', *, *, #9059, .F. ) ;
#4295 = LINE ( 'NONE', #9306, #5212 ) ;
#4296 = AXIS2_PLACEMENT_3D ( 'NONE', #10331, #2563, #7452 ) ;
#4298 = VECTOR ( 'NONE', #118, 1000.000000000000000 ) ;
#4297 = FACE_OUTER_BOUND ( 'NONE', #6825, .T. ) ;
#4299 = ORIENTED_EDGE ( 'NONE', *, *, #12320, .T. ) ;
#4300 = DIRECTION ( 'NONE',  ( 1.238279320584846685E-16, -0.9554649393887560960, 0.2951046417778627751 ) ) ;
#4301 = AXIS2_PLACEMENT_3D ( 'NONE', #1445, #12087, #4221 ) ;
#4302 = ORIENTED_EDGE ( 'NONE', *, *, #9334, .T. ) ;
#4303 = DIRECTION ( 'NONE',  ( 1.000000000000000000, -1.010728034814421376E-30, -1.090846720500930387E-30 ) ) ;
#4304 = DIRECTION ( 'NONE',  ( 0.000000000000000000, 1.530455820933490821E-32, -1.000000000000000000 ) ) ;
#4305 = CARTESIAN_POINT ( 'NONE',  ( 19.99999999999999645, -4.707829255731248885, 5.709320773864518195 ) ) ;
#4306 = VECTOR ( 'NONE', #7806, 1000.000000000000000 ) ;
#4307 = DIRECTION ( 'NONE',  ( 0.000000000000000000, 5.551115123125776539E-17, 1.000000000000000000 ) ) ;
#4308 = EDGE_CURVE ( 'NONE', #2750, #9103, #6745, .T. ) ;
#4309 = EDGE_LOOP ( 'NONE', ( #1441, #94, #1643, #437 ) ) ;
#4310 = VECTOR ( 'NONE', #12221, 1000.000000000000000 ) ;
#4311 = ORIENTED_EDGE ( 'NONE', *, *, #10751, .T. ) ;
#4312 = CARTESIAN_POINT ( 'NONE',  ( -17.00000000000000000, 30.00000000000000000, 3.000000000000030198 ) ) ;
#4313 = FACE_OUTER_BOUND ( 'NONE', #1556, .T. ) ;
#4314 = AXIS2_PLACEMENT_3D ( 'NONE', #6303, #6240, #12180 ) ;
#4315 = VECTOR ( 'NONE', #266, 1000.000000000000000 ) ;
#4316 = AXIS2_PLACEMENT_3D ( 'NONE', #1128, #2298, #8014 ) ;
#4317 = EDGE_CURVE ( 'NONE', #4933, #5731, #10790, .T. ) ;
#4318 = CYLINDRICAL_SURFACE ( 'NONE', #9682, 2.149999999999999023 ) ;
#4319 = ADVANCED_FACE ( 'NONE', ( #104 ), #6821, .T. ) ;
#4320 = CARTESIAN_POINT ( 'NONE',  ( 3.122502256758252770E-14, -4.618802153517027165, -3.433295621305388678 ) ) ;
#4321 = FACE_OUTER_BOUND ( 'NONE', #875, .T. ) ;
#4322 = DIRECTION ( 'NONE',  ( 0.000000000000000000, 0.000000000000000000, 1.000000000000000000 ) ) ;
#4323 = EDGE_LOOP ( 'NONE', ( #760, #5899, #11045, #6572 ) ) ;
#4324 = DIRECTION ( 'NONE',  ( 0.000000000000000000, 0.8345732537213000901, 0.5508969814521065267 ) ) ;
#4325 = AXIS2_PLACEMENT_3D ( 'NONE', #4745, #5703, #2893 ) ;
#4326 = CIRCLE ( 'NONE', #10890, 2.800000000000002931 ) ;
#4327 = LINE ( 'NONE', #3379, #5184 ) ;
#4328 = EDGE_CURVE ( 'NONE', #11755, #7484, #11060, .T. ) ;
#4329 = VERTEX_POINT ( 'NONE', #945 ) ;
#4330 = DIRECTION ( 'NONE',  ( 1.000000000000000000, 1.081682119347366197E-16, -6.938893903907228378E-17 ) ) ;
#4331 = CARTESIAN_POINT ( 'NONE',  ( -17.00000000000002842, -20.00000000000000000, 9.850000000000036948 ) ) ;
#4332 = STYLED_ITEM ( 'NONE', ( #7424 ), #4339 ) ;
#4333 = CARTESIAN_POINT ( 'NONE',  ( -3.999999999999993339, -2.472261339043345885, -3.687027428081202540 ) ) ;
#4334 = CYLINDRICAL_SURFACE ( 'NONE', #7543, 7.400000000000010125 ) ;
#4335 = EDGE_CURVE ( 'NONE', #5973, #6015, #1851, .T. ) ;
#4336 = DIRECTION ( 'NONE',  ( 1.000000000000000000, -1.010728034814421376E-30, -1.090846720500930387E-30 ) ) ;
#4337 = DIRECTION ( 'NONE',  ( -1.000000000000000000, 1.010728034814421376E-30, 1.090846720500930387E-30 ) ) ;
#4338 = EDGE_CURVE ( 'NONE', #1582, #6684, #1972, .T. ) ;
#4339 = ADVANCED_BREP_SHAPE_REPRESENTATION ( '', ( #1696, #12422 ), #4543 ) ;
#4340 = FILL_AREA_STYLE_COLOUR ( '', #598 ) ;
#4341 = ORIENTED_EDGE ( 'NONE', *, *, #164, .T. ) ;
#4342 = CYLINDRICAL_SURFACE ( 'NONE', #10710, 7.400000000000010125 ) ;
#4343 = EDGE_LOOP ( 'NONE', ( #3377, #3284 ) ) ;
#4344 = PRESENTATION_LAYER_ASSIGNMENT (  '', '', ( #4964 ) ) ;
#4345 = ORIENTED_EDGE ( 'NONE', *, *, #9386, .T. ) ;
#4346 = ORIENTED_EDGE ( 'NONE', *, *, #5180, .T. ) ;
#4347 = CARTESIAN_POINT ( 'NONE',  ( -1.312671235360375999, -3.860931062424216798, -0.05923475698270382062 ) ) ;
#4348 = CARTESIAN_POINT ( 'NONE',  ( 20.00000000000000355, 18.52447679111067913, -16.77732469694377926 ) ) ;
#4349 = CARTESIAN_POINT ( 'NONE',  ( -35.00000000000006395, -19.99999999999999645, 3.000000000000008438 ) ) ;
#4350 = DIRECTION ( 'NONE',  ( -1.000000000000000000, 1.010728034814421376E-30, 1.090846720500930387E-30 ) ) ;
#4351 = EDGE_CURVE ( 'NONE', #5322, #2127, #5773, .T. ) ;
#4352 = FACE_OUTER_BOUND ( 'NONE', #4551, .T. ) ;
#4353 = ORIENTED_EDGE ( 'NONE', *, *, #9491, .F. ) ;
#4354 = DIRECTION ( 'NONE',  ( -1.031065855027150586E-29, 1.000000000000000000, 6.695352868347756765E-17 ) ) ;
#4355 = DIRECTION ( 'NONE',  ( -1.577021341797098546E-16, -1.177425296209237084E-30, -1.000000000000000000 ) ) ;
#4356 = VERTEX_POINT ( 'NONE', #12747 ) ;
#4357 = ORIENTED_EDGE ( 'NONE', *, *, #1282, .T. ) ;
#4358 = EDGE_CURVE ( 'NONE', #9929, #5919, #9594, .T. ) ;
#4359 = ORIENTED_EDGE ( 'NONE', *, *, #9569, .T. ) ;
#4360 = EDGE_CURVE ( 'NONE', #1611, #3455, #7741, .T. ) ;
#4361 = ORIENTED_EDGE ( 'NONE', *, *, #8762, .F. ) ;
#4362 = DIRECTION ( 'NONE',  ( -1.000000000000000000, 1.010728034814421376E-30, 1.090846720500930387E-30 ) ) ;
#4363 = AXIS2_PLACEMENT_3D ( 'NONE', #5104, #2008, #977 ) ;
#4364 = CARTESIAN_POINT ( 'NONE',  ( -9.860132971832690885, -30.00000000000000000, -1.666666666666667629 ) ) ;
#4365 = ORIENTED_EDGE ( 'NONE', *, *, #12034, .T. ) ;
#4366 = APPLICATION_CONTEXT ( 'automotive_design' ) ;
#4367 = DIRECTION ( 'NONE',  ( 0.000000000000000000, -0.9195277725514543476, 0.3930250316539146693 ) ) ;
#4368 = ORIENTED_EDGE ( 'NONE', *, *, #3155, .F. ) ;
#4369 = DIRECTION ( 'NONE',  ( 0.000000000000000000, 0.000000000000000000, -1.000000000000000000 ) ) ;
#4370 = DIRECTION ( 'NONE',  ( 0.000000000000000000, 1.000000000000000000, 0.000000000000000000 ) ) ;
#4371 = CLOSED_SHELL ( 'NONE', ( #9615, #5836, #3611, #2847, #7179, #7071, #56, #966, #11280, #2403, #4286, #6045, #11328, #3825, #10066, #9186, #6828, #4630, #6036, #3066, #10927, #9412, #2598, #12044, #4874, #3655, #5412 ) ) ;
#4372 = DIRECTION ( 'NONE',  ( -1.000000000000000000, 1.010728034814421376E-30, 1.090846720500930387E-30 ) ) ;
#4373 = AXIS2_PLACEMENT_3D ( 'NONE', #253, #4188, #8178 ) ;
#4374 = DIRECTION ( 'NONE',  ( 0.000000000000000000, 0.9749279121818227312, 0.2225209339563182787 ) ) ;
#4375 = ORIENTED_EDGE ( 'NONE', *, *, #8905, .T. ) ;
#4376 = PRODUCT_DEFINITION ( 'UNKNOWN', '', #1585, #1990 ) ;
#4377 = ORIENTED_EDGE ( 'NONE', *, *, #9013, .T. ) ;
#4378 = DIRECTION ( 'NONE',  ( -1.159061634649218351E-16, 0.000000000000000000, -1.000000000000000000 ) ) ;
#4379 = VECTOR ( 'NONE', #5234, 1000.000000000000000 ) ;
#4380 = CARTESIAN_POINT ( 'NONE',  ( -4.000000000000001776, 2.309401076758498039, -0.4999999999999935052 ) ) ;
#4381 = CIRCLE ( 'NONE', #258, 6.999999999999999112 ) ;
#4382 = DIRECTION ( 'NONE',  ( 0.000000000000000000, 0.000000000000000000, 1.000000000000000000 ) ) ;
#4383 = ADVANCED_FACE ( 'NONE', ( #12685, #8924 ), #4031, .T. ) ;
#4384 = DIRECTION ( 'NONE',  ( -1.238279320584846685E-16, 0.9554649393887558739, -0.2951046417778634412 ) ) ;
#4385 = CARTESIAN_POINT ( 'NONE',  ( 2.000000000000001776, 1.773042676681341856, -3.469446951953614189E-15 ) ) ;
#4386 = AXIS2_PLACEMENT_3D ( 'NONE', #9937, #1132, #3217 ) ;
#4387 = CARTESIAN_POINT ( 'NONE',  ( 40.00000000000006395, 4.500000000000000000, -20.00000000000000000 ) ) ;
#4388 = ORIENTED_EDGE ( 'NONE', *, *, #4600, .F. ) ;
#4389 = B_SPLINE_CURVE_WITH_KNOTS ( 'NONE', 3,
 ( #9662, #10699, #2939, #4603, #8518 ),
 .UNSPECIFIED., .F., .F.,
 ( 4, 1, 4 ),
 ( 0.000000000000000000, 0.002309401076758505790, 0.004618802153517011580 ),
 .UNSPECIFIED. ) ;
#4390 = CARTESIAN_POINT ( 'NONE',  ( 3.540020015735469983, 2.810662092924230304, -3.602146406945803125 ) ) ;
#4391 = ADVANCED_FACE ( 'NONE', ( #10854 ), #2035, .T. ) ;
#4392 = DIRECTION ( 'NONE',  ( -1.000000000000000000, -5.916456789157575403E-31, 1.577021341797098793E-16 ) ) ;
#4393 = EDGE_CURVE ( 'NONE', #9120, #3923, #3265, .T. ) ;
#4394 = AXIS2_PLACEMENT_3D ( 'NONE', #208, #4139, #8056 ) ;
#4395 = VERTEX_POINT ( 'NONE', #8861 ) ;
#4396 = CARTESIAN_POINT ( 'NONE',  ( 6.000000000000000000, 49.63999999999998636, -17.00000000000000000 ) ) ;
#4397 = ADVANCED_FACE ( 'NONE', ( #2905 ), #8802, .T. ) ;
#4398 = DIRECTION ( 'NONE',  ( 0.000000000000000000, 0.000000000000000000, 1.000000000000000000 ) ) ;
#4399 = CARTESIAN_POINT ( 'NONE',  ( -10.00000000000000178, 0.000000000000000000, 0.000000000000000000 ) ) ;
#4400 = DIRECTION ( 'NONE',  ( 0.000000000000000000, 0.000000000000000000, -1.000000000000000000 ) ) ;
#4401 = CARTESIAN_POINT ( 'NONE',  ( 11.00000000000003375, -6.123233995736748533E-16, 17.85000000000004405 ) ) ;
#4402 = DIRECTION ( 'NONE',  ( -1.000000000000000000, 1.010728034814421376E-30, 1.090846720500930387E-30 ) ) ;
#4403 = CARTESIAN_POINT ( 'NONE',  ( 20.00000000000000000, 10.64574963035789601, -21.19875926443459591 ) ) ;
#4404 = CIRCLE ( 'NONE', #9325, 3.500000000000003997 ) ;
#4405 = ORIENTED_EDGE ( 'NONE', *, *, #840, .T. ) ;
#4406 = CARTESIAN_POINT ( 'NONE',  ( 20.00000000000006750, 4.499999999999998224, -20.00000000000000000 ) ) ;
#4407 = ORIENTED_EDGE ( 'NONE', *, *, #4002, .T. ) ;
#4408 = ORIENTED_EDGE ( 'NONE', *, *, #5789, .F. ) ;
#4409 = CONTEXT_DEPENDENT_SHAPE_REPRESENTATION ( #6591, #3796 ) ;
#4410 = ORIENTED_EDGE ( 'NONE', *, *, #2441, .F. ) ;
#4411 = TOROIDAL_SURFACE ( 'NONE', #2140, 5.384454397937118664, 0.5155456020628804703 ) ;
#4412 = VERTEX_POINT ( 'NONE', #3915 ) ;
#4413 = CYLINDRICAL_SURFACE ( 'NONE', #2967, 6.499000000000010324 ) ;
#4414 = DIRECTION ( 'NONE',  ( 1.000000000000000000, 1.081682119347366197E-16, -6.938893903907228378E-17 ) ) ;
#4415 = CARTESIAN_POINT ( 'NONE',  ( 40.00000000000000711, 18.52447679111068268, -16.77732469694377926 ) ) ;
#4416 = CARTESIAN_POINT ( 'NONE',  ( 0.000000000000000000, 7.100173756228419286, 2.085073771204575710 ) ) ;
#4417 = VERTEX_POINT ( 'NONE', #4944 ) ;
#4418 = DIRECTION ( 'NONE',  ( 0.000000000000000000, 0.5000000000000012212, 0.8660254037844380415 ) ) ;
#4419 = FACE_OUTER_BOUND ( 'NONE', #9756, .T. ) ;
#4420 = ORIENTED_EDGE ( 'NONE', *, *, #2432, .F. ) ;
#4421 = AXIS2_PLACEMENT_3D ( 'NONE', #5787, #11726, #9700 ) ;
#4422 = AXIS2_PLACEMENT_3D ( 'NONE', #7008, #4032, #2036 ) ;
#4423 = ORIENTED_EDGE ( 'NONE', *, *, #2624, .F. ) ;
#4424 = EDGE_LOOP ( 'NONE', ( #3750, #2234, #2503, #10653 ) ) ;
#4425 = ORIENTED_EDGE ( 'NONE', *, *, #2439, .F. ) ;
#4426 = LINE ( 'NONE', #8351, #3574 ) ;
#4427 = PRODUCT ( 'upper roller_ISO - Spur gear 0.4M 35T 20PA 20FW ---S35A75H50L5.0N', 'upper roller_ISO - Spur gear 0.4M 35T 20PA 20FW ---S35A75H50L5.0N', '', ( #1125 ) ) ;
#4428 = DIRECTION ( 'NONE',  ( 0.000000000000000000, -1.530455820933490821E-32, 1.000000000000000000 ) ) ;
#4429 = ORIENTED_EDGE ( 'NONE', *, *, #2359, .T. ) ;
#4430 = DIRECTION ( 'NONE',  ( -1.140150527077241873E-30, 0.000000000000000000, 1.000000000000000000 ) ) ;
#4431 = ORIENTED_EDGE ( 'NONE', *, *, #2244, .F. ) ;
#4432 = AXIS2_PLACEMENT_3D ( 'NONE', #3545, #6365, #7464 ) ;
#4433 = AXIS2_PLACEMENT_3D ( 'NONE', #1707, #6549, #7636 ) ;
#4434 = DIRECTION ( 'NONE',  ( 0.000000000000000000, 0.000000000000000000, -1.000000000000000000 ) ) ;
#4435 = EDGE_CURVE ( 'NONE', #1618, #9867, #7839, .T. ) ;
#4436 = SHAPE_REPRESENTATION ( 'socket head cap screw_iso_ISO 4762 M4 x 25 - 25N', ( #12422 ), #7637 ) ;
#4437 = DIRECTION ( 'NONE',  ( 0.000000000000000000, 0.000000000000000000, 1.000000000000000000 ) ) ;
#4438 = DIRECTION ( 'NONE',  ( 1.140150527077241873E-30, 0.000000000000000000, -1.000000000000000000 ) ) ;
#4439 = PRODUCT_DEFINITION_CONTEXT ( 'detailed design', #5674, 'design' ) ;
#4440 = DIRECTION ( 'NONE',  ( -1.000000000000000000, 1.010728034814421376E-30, 1.090846720500930387E-30 ) ) ;
#4441 = ORIENTED_EDGE ( 'NONE', *, *, #7038, .T. ) ;
#4442 = ORIENTED_EDGE ( 'NONE', *, *, #4049, .T. ) ;
#4443 = AXIS2_PLACEMENT_3D ( 'NONE', #6327, #1432, #5364 ) ;
#4444 = FACE_OUTER_BOUND ( 'NONE', #8973, .T. ) ;
#4445 =( NAMED_UNIT ( * ) SI_UNIT ( $, .STERADIAN. ) SOLID_ANGLE_UNIT ( ) );
#4446 = CARTESIAN_POINT ( 'NONE',  ( -4.207491450040580894, 2.029819825146461199, -3.671670828759564742 ) ) ;
#4447 = CARTESIAN_POINT ( 'NONE',  ( -1.317756351988342400, 3.857995168970202116, -0.04852650426601479161 ) ) ;
#4448 = EDGE_CURVE ( 'NONE', #12527, #955, #7960, .T. ) ;
#4449 = CARTESIAN_POINT ( 'NONE',  ( 4.000000000000002665, -0.8578082829537354570, -3.433262215449998322 ) ) ;
#4450 = AXIS2_PLACEMENT_3D ( 'NONE', #2235, #6152, #3152 ) ;
#4451 = PLANE ( 'NONE',  #1743 ) ;
#4452 = DIRECTION ( 'NONE',  ( 0.000000000000000000, -0.8805955318567322276, -0.4738686624730095165 ) ) ;
#4453 = ORIENTED_EDGE ( 'NONE', *, *, #4002, .F. ) ;
#4454 = CARTESIAN_POINT ( 'NONE',  ( 0.5636800770131545901, 4.293361309317545782, -3.531542292954619633 ) ) ;
#4455 = EDGE_CURVE ( 'NONE', #10836, #1407, #8583, .T. ) ;
#4456 = CARTESIAN_POINT ( 'NONE',  ( 0.000000000000000000, 0.000000000000000000, 0.000000000000000000 ) ) ;
#4457 =( LENGTH_UNIT ( ) NAMED_UNIT ( * ) SI_UNIT ( .MILLI., .METRE. ) );
#4458 = MECHANICAL_DESIGN_GEOMETRIC_PRESENTATION_REPRESENTATION (  '', ( #7344 ), #10617 ) ;
#4459 = CARTESIAN_POINT ( 'NONE',  ( 0.000000000000000000, 0.000000000000000000, 0.000000000000000000 ) ) ;
#4460 = ORIENTED_EDGE ( 'NONE', *, *, #1749, .F. ) ;
#4461 = CARTESIAN_POINT ( 'NONE',  ( 19.99999999999997868, 6.544726022087268724, -0.6592800351836389794 ) ) ;
#4462 = DIRECTION ( 'NONE',  ( 1.000000000000000000, -1.010728034814421376E-30, -1.090846720500930387E-30 ) ) ;
#4463 = CARTESIAN_POINT ( 'NONE',  ( 14.00000000000000000, -30.00000000000000000, 4.000000000000000000 ) ) ;
#4464 = EDGE_CURVE ( 'NONE', #479, #5907, #151, .T. ) ;
#4465 = CARTESIAN_POINT ( 'NONE',  ( 3.861362476283253464, 2.629030857715976222, -3.671615880910352292 ) ) ;
#4466 = DIRECTION ( 'NONE',  ( 1.000000000000000000, -0.000000000000000000, -6.938893903907228378E-17 ) ) ;
#4467 = AXIS2_PLACEMENT_3D ( 'NONE', #7594, #2722, #5657 ) ;
#4468 = EDGE_CURVE ( 'NONE', #8054, #11067, #8985, .T. ) ;
#4469 = VECTOR ( 'NONE', #8952, 1000.000000000000000 ) ;
#4470 = LINE ( 'NONE', #8390, #8315 ) ;
#4471 = AXIS2_PLACEMENT_3D ( 'NONE', #1301, #2217, #9154 ) ;
#4472 = CARTESIAN_POINT ( 'NONE',  ( 2.000000000000001776, -1.773042676681348739, 1.387778780781445676E-14 ) ) ;
#4473 = EDGE_CURVE ( 'NONE', #9408, #412, #12100, .T. ) ;
#4474 = CARTESIAN_POINT ( 'NONE',  ( 11.00000000000002665, 12.50000000000000000, -6.000000000000017764 ) ) ;
#4475 = ORIENTED_EDGE ( 'NONE', *, *, #3460, .F. ) ;
#4476 = ITEM_DEFINED_TRANSFORMATION ( 'NONE', 'NONE', #965,  #12422 ) ;
#4477 = ORIENTED_EDGE ( 'NONE', *, *, #4523, .F. ) ;
#4478 = ORIENTED_EDGE ( 'NONE', *, *, #7288, .F. ) ;
#4479 = VECTOR ( 'NONE', #8422, 1000.000000000000000 ) ;
#4480 = CARTESIAN_POINT ( 'NONE',  ( 9.999999999999998224, 5.025702764809159895, -5.431603052487340655 ) ) ;
#4481 = PRESENTATION_STYLE_ASSIGNMENT (( #9352 ) ) ;
#4482 = DIRECTION ( 'NONE',  ( 0.000000000000000000, 0.000000000000000000, 1.000000000000000000 ) ) ;
#4483 = EDGE_CURVE ( 'NONE', #9770, #5717, #975, .T. ) ;
#4484 = DIRECTION ( 'NONE',  ( -1.000000000000000000, 1.010728034814421376E-30, 1.090846720500930387E-30 ) ) ;
#4485 = ORIENTED_EDGE ( 'NONE', *, *, #706, .T. ) ;
#4486 = EDGE_CURVE ( 'NONE', #2488, #12421, #10210, .T. ) ;
#4487 = CARTESIAN_POINT ( 'NONE',  ( 19.99999999999999645, 0.000000000000000000, 0.000000000000000000 ) ) ;
#4488 = CARTESIAN_POINT ( 'NONE',  ( -40.00000000000000000, 30.00000000000000000, 2.831145448779744488E-15 ) ) ;
#4489 = VERTEX_POINT ( 'NONE', #8022 ) ;
#4490 = VERTEX_POINT ( 'NONE', #6283 ) ;
#4491 = CARTESIAN_POINT ( 'NONE',  ( 11.00000000000003020, 30.00000000000000000, 25.00000000000007105 ) ) ;
#4492 = ORIENTED_EDGE ( 'NONE', *, *, #696, .F. ) ;
#4493 = VERTEX_POINT ( 'NONE', #8150 ) ;
#4494 = CARTESIAN_POINT ( 'NONE',  ( 40.00000000000000000, 39.34792583643766051, -17.06347054209567915 ) ) ;
#4495 = FACE_OUTER_BOUND ( 'NONE', #12217, .T. ) ;
#4496 = ORIENTED_EDGE ( 'NONE', *, *, #1394, .F. ) ;
#4497 = CARTESIAN_POINT ( 'NONE',  ( 0.000000000000000000, 1.528443194675508376, -7.240432404259457222 ) ) ;
#4498 = DIRECTION ( 'NONE',  ( 0.000000000000000000, 0.000000000000000000, 1.000000000000000000 ) ) ;
#4499 = VERTEX_POINT ( 'NONE', #10131 ) ;
#4500 = DIRECTION ( 'NONE',  ( -1.000000000000000000, 1.010728034814421376E-30, 1.090846720500930387E-30 ) ) ;
#4501 = DIRECTION ( 'NONE',  ( -1.000000000000000000, 1.010728034814421376E-30, 1.090846720500930387E-30 ) ) ;
#4502 = VECTOR ( 'NONE', #8839, 1000.000000000000227 ) ;
#4503 = EDGE_CURVE ( 'NONE', #4277, #11776, #1996, .T. ) ;
#4504 = DIRECTION ( 'NONE',  ( -1.848892746611746419E-31, -1.000000000000000000, 3.250006781153460502E-32 ) ) ;
#4505 = DIRECTION ( 'NONE',  ( -0.000000000000000000, 1.530455820933490821E-32, -1.000000000000000000 ) ) ;
#4506 = EDGE_CURVE ( 'NONE', #2782, #11454, #4094, .T. ) ;
#4507 = VERTEX_POINT ( 'NONE', #2237 ) ;
#4508 = VERTEX_POINT ( 'NONE', #9170 ) ;
#4509 = DIRECTION ( 'NONE',  ( 0.000000000000000000, 5.551115123125776539E-17, 1.000000000000000000 ) ) ;
#4510 = CIRCLE ( 'NONE', #10871, 2.800000000000004263 ) ;
#4511 = CARTESIAN_POINT ( 'NONE',  ( 0.000000000000000000, 6.424561140605096199, -0.9808237102696265586 ) ) ;
#4512 = FACE_OUTER_BOUND ( 'NONE', #697, .T. ) ;
#4513 = AXIS2_PLACEMENT_3D ( 'NONE', #10931, #1204, #11980 ) ;
#4514 = AXIS2_PLACEMENT_3D ( 'NONE', #8971, #8004, #1958 ) ;
#4515 = CARTESIAN_POINT ( 'NONE',  ( 40.00000000000000711, 19.99999999999999645, -12.00000000000000178 ) ) ;
#4516 = CARTESIAN_POINT ( 'NONE',  ( 0.000000000000000000, -6.413745496774120092, 3.691052519622234129 ) ) ;
#4517 = ORIENTED_EDGE ( 'NONE', *, *, #11869, .T. ) ;
#4518 = DIRECTION ( 'NONE',  ( 0.000000000000000000, 0.7227948638273878901, 0.6910626489868685329 ) ) ;
#4519 = DIRECTION ( 'NONE',  ( 8.135128085091670230E-31, 0.1785568947986370392, -0.9839295885986295565 ) ) ;
#4520 = EDGE_CURVE ( 'NONE', #11190, #12693, #3221, .T. ) ;
#4521 = ADVANCED_FACE ( 'NONE', ( #2370 ), #11056, .F. ) ;
#4522 = CIRCLE ( 'NONE', #6366, 7.400000000000009237 ) ;
#4523 = EDGE_CURVE ( 'NONE', #7265, #3948, #11899, .T. ) ;
#4524 = AXIS2_PLACEMENT_3D ( 'NONE', #976, #5227, #8255 ) ;
#4525 = AXIS2_PLACEMENT_3D ( 'NONE', #9335, #10561, #9522 ) ;
#4526 = ADVANCED_FACE ( 'NONE', ( #1193, #6154 ), #2106, .F. ) ;
#4527 = CARTESIAN_POINT ( 'NONE',  ( 4.000000000000019540, -2.309401076758522464, -3.433295621305367806 ) ) ;
#4528 = VERTEX_POINT ( 'NONE', #1257 ) ;
#4529 = CARTESIAN_POINT ( 'NONE',  ( -40.00000000000000000, -19.99999999999999645, 2.000000000000003109 ) ) ;
#4530 = LINE ( 'NONE', #10371, #6250 ) ;
#4531 = CARTESIAN_POINT ( 'NONE',  ( 14.00000000000000000, 30.00000000000000000, 4.000000000000000000 ) ) ;
#4532 = CARTESIAN_POINT ( 'NONE',  ( 2.500000000000000444, -3.469446951953614189E-14, -25.03750572909320837 ) ) ;
#4533 = DIRECTION ( 'NONE',  ( 0.000000000000000000, -1.000000000000000000, 0.000000000000000000 ) ) ;
#4534 = CIRCLE ( 'NONE', #2908, 7.400000000000009237 ) ;
#4535 = AXIS2_PLACEMENT_3D ( 'NONE', #9705, #7026, #2984 ) ;
#4536 = AXIS2_PLACEMENT_3D ( 'NONE', #11343, #5660, #3489 ) ;
#4537 = DIRECTION ( 'NONE',  ( -1.000000000000000000, 1.010728034814421376E-30, 1.090846720500930387E-30 ) ) ;
#4538 = PRODUCT ( 'ring', 'ring', '', ( #10781 ) ) ;
#4539 = FACE_OUTER_BOUND ( 'NONE', #7495, .T. ) ;
#4540 = DIRECTION ( 'NONE',  ( 0.000000000000000000, 0.000000000000000000, 1.000000000000000000 ) ) ;
#4541 = ORIENTED_EDGE ( 'NONE', *, *, #10166, .F. ) ;
#4542 = EDGE_CURVE ( 'NONE', #3396, #8673, #7006, .T. ) ;
#4543 =( GEOMETRIC_REPRESENTATION_CONTEXT ( 3 ) GLOBAL_UNCERTAINTY_ASSIGNED_CONTEXT ( ( #10481 ) ) GLOBAL_UNIT_ASSIGNED_CONTEXT ( ( #3192, #9086, #2342 ) ) REPRESENTATION_CONTEXT ( 'NONE', 'WORKASPACE' ) );
#4544 = CIRCLE ( 'NONE', #1238, 4.499999999999999112 ) ;
#4545 = ORIENTED_EDGE ( 'NONE', *, *, #2074, .F. ) ;
#4546 = ORIENTED_EDGE ( 'NONE', *, *, #4790, .F. ) ;
#4547 = DIRECTION ( 'NONE',  ( 1.224646799147353207E-16, 1.000000000000000000, 1.530455820933490821E-32 ) ) ;
#4548 = SURFACE_STYLE_FILL_AREA ( #1510 ) ;
#4549 = DIRECTION ( 'NONE',  ( -0.000000000000000000, -1.000000000000000000, -0.000000000000000000 ) ) ;
#4550 = CARTESIAN_POINT ( 'NONE',  ( 2.000000000000001776, -1.773042676681348739, 1.387778780781445676E-14 ) ) ;
#4551 = EDGE_LOOP ( 'NONE', ( #1395, #8552, #11834, #1977 ) ) ;
#4552 = EDGE_CURVE ( 'NONE', #4276, #8365, #10987, .T. ) ;
#4553 = LINE ( 'NONE', #11380, #11841 ) ;
#4554 = MECHANICAL_DESIGN_GEOMETRIC_PRESENTATION_REPRESENTATION (  '', ( #8033 ), #5361 ) ;
#4555 = CARTESIAN_POINT ( 'NONE',  ( 0.000000000000000000, -1.113123845672418177, 7.315801754025009096 ) ) ;
#4556 = ORIENTED_EDGE ( 'NONE', *, *, #9984, .F. ) ;
#4557 = ORIENTED_EDGE ( 'NONE', *, *, #877, .F. ) ;
#4558 = DIRECTION ( 'NONE',  ( 1.000000000000000000, 1.031065855027150586E-29, 2.218671295934092550E-30 ) ) ;
#4559 = EDGE_LOOP ( 'NONE', ( #1149, #10605, #6760, #9597 ) ) ;
#4560 = EDGE_LOOP ( 'NONE', ( #8725, #2308, #10016, #5358 ) ) ;
#4561 = EDGE_CURVE ( 'NONE', #7169, #4507, #4226, .T. ) ;
#4562 = ADVANCED_FACE ( 'NONE', ( #10918 ), #3281, .T. ) ;
#4563 = CARTESIAN_POINT ( 'NONE',  ( 19.99999999999997868, 2.796709610837448068, -6.851161606081828559 ) ) ;
#4564 = ORIENTED_EDGE ( 'NONE', *, *, #5409, .T. ) ;
#4565 = DIRECTION ( 'NONE',  ( -1.000000000000000000, 1.010728034814421376E-30, 1.090846720500930387E-30 ) ) ;
#4566 = DIRECTION ( 'NONE',  ( -1.000000000000000000, 1.010728034814421376E-30, 1.090846720500930387E-30 ) ) ;
#4567 = AXIS2_PLACEMENT_3D ( 'NONE', #5060, #11107, #6209 ) ;
#4568 = VERTEX_POINT ( 'NONE', #5379 ) ;
#4569 = FACE_OUTER_BOUND ( 'NONE', #11301, .T. ) ;
#4570 = LINE ( 'NONE', #8548, #3200 ) ;
#4571 = LINE ( 'NONE', #3669, #8333 ) ;
#4572 = CIRCLE ( 'NONE', #247, 7.400000000000009237 ) ;
#4573 = CARTESIAN_POINT ( 'NONE',  ( 0.000000000000000000, 0.000000000000000000, 0.000000000000000000 ) ) ;
#4574 = ORIENTED_EDGE ( 'NONE', *, *, #11571, .T. ) ;
#4575 = AXIS2_PLACEMENT_3D ( 'NONE', #10891, #5997, #4977 ) ;
#4576 = EDGE_LOOP ( 'NONE', ( #1184, #2704, #11370, #2970 ) ) ;
#4577 = DIRECTION ( 'NONE',  ( 1.000000000000000000, 0.000000000000000000, 0.000000000000000000 ) ) ;
#4578 = DIRECTION ( 'NONE',  ( 1.000000000000000000, 0.000000000000000000, 0.000000000000000000 ) ) ;
#4579 = ORIENTED_EDGE ( 'NONE', *, *, #1787, .T. ) ;
#4580 = LINE ( 'NONE', #702, #3722 ) ;
#4581 = CARTESIAN_POINT ( 'NONE',  ( 4.000000000000003553, 0.000000000000000000, 0.000000000000000000 ) ) ;
#4582 = ADVANCED_FACE ( 'NONE', ( #4352 ), #3526, .T. ) ;
#4583 = CIRCLE ( 'NONE', #3150, 0.2000000000000000944 ) ;
#4584 = DIRECTION ( 'NONE',  ( -1.000000000000000000, 0.000000000000000000, 0.000000000000000000 ) ) ;
#4585 = DIRECTION ( 'NONE',  ( 0.000000000000000000, 5.551115123125776539E-17, 1.000000000000000000 ) ) ;
#4586 = EDGE_LOOP ( 'NONE', ( #6506, #2383, #10324 ) ) ;
#4587 = CARTESIAN_POINT ( 'NONE',  ( 0.000000000000000000, 6.359055127044389799, 1.682410996215986998 ) ) ;
#4588 = CIRCLE ( 'NONE', #10542, 2.149999999999994138 ) ;
#4589 = CARTESIAN_POINT ( 'NONE',  ( 19.99999999999999645, 4.772487208025126826, 4.411390579991361527 ) ) ;
#4590 = CIRCLE ( 'NONE', #10333, 2.800000000000004263 ) ;
#4591 = DIRECTION ( 'NONE',  ( -1.000000000000000000, 1.010728034814421376E-30, 1.090846720500930387E-30 ) ) ;
#4592 = VERTEX_POINT ( 'NONE', #11311 ) ;
#4593 = DIRECTION ( 'NONE',  ( -1.000000000000000000, 0.000000000000000000, 0.000000000000000000 ) ) ;
#4594 = DIRECTION ( 'NONE',  ( 1.000000000000000000, -0.000000000000000000, -6.938893903907228378E-17 ) ) ;
#4595 = CIRCLE ( 'NONE', #9509, 2.800000000000003819 ) ;
#4596 = DIRECTION ( 'NONE',  ( -1.031065855027149465E-29, -1.000000000000000000, 7.771561172376086908E-16 ) ) ;
#4597 = CARTESIAN_POINT ( 'NONE',  ( 1.391697335622807952, 4.043246145443367467, -3.503898532754372130 ) ) ;
#4598 = EDGE_CURVE ( 'NONE', #271, #10402, #2621, .T. ) ;
#4599 = DIRECTION ( 'NONE',  ( 1.000000000000000000, 0.000000000000000000, 0.000000000000000000 ) ) ;
#4600 = EDGE_CURVE ( 'NONE', #2451, #1427, #12472, .T. ) ;
#4601 = LINE ( 'NONE', #8514, #11819 ) ;
#4602 = DIRECTION ( 'NONE',  ( 0.000000000000000000, -1.530455820933490821E-32, 1.000000000000000000 ) ) ;
#4603 = CARTESIAN_POINT ( 'NONE',  ( -3.999999999999964473, -1.539600717839013422, -3.300726591567098023 ) ) ;
#4604 = EDGE_LOOP ( 'NONE', ( #7254, #8728, #11317, #8154 ) ) ;
#4605 = VECTOR ( 'NONE', #4795, 1000.000000000000000 ) ;
#4606 = VERTEX_POINT ( 'NONE', #12285 ) ;
#4607 = ORIENTED_EDGE ( 'NONE', *, *, #7208, .F. ) ;
#4608 = CARTESIAN_POINT ( 'NONE',  ( 19.99999999999999645, 2.796709610837343707, 6.851161606081852540 ) ) ;
#4609 = CARTESIAN_POINT ( 'NONE',  ( 19.99999999999999645, -1.623118704078951202, 6.293050665016855838 ) ) ;
#4610 = DIRECTION ( 'NONE',  ( 1.000000000000000000, -1.010728034814421376E-30, -1.090846720500930387E-30 ) ) ;
#4611 = LINE ( 'NONE', #3649, #8149 ) ;
#4612 = ORIENTED_EDGE ( 'NONE', *, *, #7383, .T. ) ;
#4613 = DIRECTION ( 'NONE',  ( -1.000000000000000000, 1.010728034814421376E-30, 1.090846720500930387E-30 ) ) ;
#4614 = EDGE_CURVE ( 'NONE', #8175, #9475, #3588, .T. ) ;
#4615 = DIRECTION ( 'NONE',  ( 0.000000000000000000, 0.9909497617679352555, -0.1342332658176522697 ) ) ;
#4616 = ORIENTED_EDGE ( 'NONE', *, *, #12238, .F. ) ;
#4617 = ORIENTED_EDGE ( 'NONE', *, *, #5824, .T. ) ;
#4618 = CARTESIAN_POINT ( 'NONE',  ( -15.00000000000000000, 30.00000000000000000, 3.000000000000029754 ) ) ;
#4619 = EDGE_LOOP ( 'NONE', ( #4341, #12276 ) ) ;
#4620 = ORIENTED_EDGE ( 'NONE', *, *, #5186, .T. ) ;
#4621 = AXIS2_PLACEMENT_3D ( 'NONE', #12729, #11822, #9736 ) ;
#4622 = CARTESIAN_POINT ( 'NONE',  ( 3.469446951953614189E-14, -3.469446951953614189E-15, -4.484454397937126302 ) ) ;
#4623 = ORIENTED_EDGE ( 'NONE', *, *, #2051, .T. ) ;
#4624 = FACE_OUTER_BOUND ( 'NONE', #7011, .T. ) ;
#4625 = CYLINDRICAL_SURFACE ( 'NONE', #5542, 2.800000000000003819 ) ;
#4626 = VERTEX_POINT ( 'NONE', #4416 ) ;
#4627 = FACE_OUTER_BOUND ( 'NONE', #2711, .T. ) ;
#4628 = DIRECTION ( 'NONE',  ( -1.000000000000000000, 1.010728034814421376E-30, 1.090846720500930387E-30 ) ) ;
#4629 = CIRCLE ( 'NONE', #10779, 4.000000000000000000 ) ;
#4630 = ADVANCED_FACE ( 'NONE', ( #8464 ), #3404, .T. ) ;
#4631 = AXIS2_PLACEMENT_3D ( 'NONE', #6502, #2781, #6632 ) ;
#4632 = CARTESIAN_POINT ( 'NONE',  ( 19.99999999999999645, -4.907279493584762342, 4.380262188593320616 ) ) ;
#4633 = EDGE_CURVE ( 'NONE', #8204, #11065, #11455, .T. ) ;
#4634 = ORIENTED_EDGE ( 'NONE', *, *, #10414, .F. ) ;
#4635 = ORIENTED_EDGE ( 'NONE', *, *, #11903, .T. ) ;
#4636 = DIRECTION ( 'NONE',  ( 0.000000000000000000, 1.000000000000000000, 0.000000000000000000 ) ) ;
#4637 = ADVANCED_FACE ( 'NONE', ( #6547 ), #2696, .T. ) ;
#4638 = AXIS2_PLACEMENT_3D ( 'NONE', #7525, #440, #9314 ) ;
#4639 = DIRECTION ( 'NONE',  ( -1.000000000000000000, -2.891205793294675861E-16, -3.658689512969251529E-17 ) ) ;
#4640 = ORIENTED_EDGE ( 'NONE', *, *, #3203, .F. ) ;
#4641 = AXIS2_PLACEMENT_3D ( 'NONE', #11442, #12353, #4741 ) ;
#4642 = CARTESIAN_POINT ( 'NONE',  ( 27.00000000000000355, 40.41548023366552655, -10.14535464186970337 ) ) ;
#4643 = CARTESIAN_POINT ( 'NONE',  ( 15.00000000000003375, -12.49999999999999645, 6.000000000000000000 ) ) ;
#4644 = PRODUCT_DEFINITION_SHAPE ( 'NONE', 'NONE',  #2904 ) ;
#4645 = CARTESIAN_POINT ( 'NONE',  ( 0.000000000000000000, -2.720702104307052949, 5.902099716170440047 ) ) ;
#4646 = VECTOR ( 'NONE', #3635, 1000.000000000000000 ) ;
#4647 = FACE_OUTER_BOUND ( 'NONE', #9678, .T. ) ;
#4648 = ORIENTED_EDGE ( 'NONE', *, *, #1706, .T. ) ;
#4649 = FACE_OUTER_BOUND ( 'NONE', #1860, .T. ) ;
#4650 = ORIENTED_EDGE ( 'NONE', *, *, #9514, .F. ) ;
#4651 = CARTESIAN_POINT ( 'NONE',  ( -3.999999999999963585, -2.309401076758515359, -3.504269196027888889 ) ) ;
#4652 = CARTESIAN_POINT ( 'NONE',  ( 19.99999999999997868, 6.359055127044406674, -1.682410996215896848 ) ) ;
#4653 = DIRECTION ( 'NONE',  ( -1.000000000000000000, 0.000000000000000000, 0.000000000000000000 ) ) ;
#4654 = CIRCLE ( 'NONE', #11027, 6.499000000000009436 ) ;
#4655 = CARTESIAN_POINT ( 'NONE',  ( 27.00000000000001066, 58.55522666905708462, -36.77936687539386185 ) ) ;
#4656 = DIRECTION ( 'NONE',  ( -0.7071067811865355823, 8.659560562355079537E-17, -0.7071067811865595631 ) ) ;
#4657 = CARTESIAN_POINT ( 'NONE',  ( 0.000000000000000000, -2.099089055167725704, -6.233932467347810480 ) ) ;
#4658 = CARTESIAN_POINT ( 'NONE',  ( 0.000000000000000000, -2.171317488608555557, 7.074275960383694439 ) ) ;
#4659 = CARTESIAN_POINT ( 'NONE',  ( 13.63191942669736889, -12.49999999999999645, 3.758770483143645702 ) ) ;
#4660 = ADVANCED_FACE ( 'NONE', ( #7445 ), #6613, .F. ) ;
#4661 = DIRECTION ( 'NONE',  ( -3.437775699846489820E-17, -0.2951046417778627751, -0.9554649393887560960 ) ) ;
#4662 = AXIS2_PLACEMENT_3D ( 'NONE', #10583, #3524, #11375 ) ;
#4663 = CARTESIAN_POINT ( 'NONE',  ( 14.00000000000000000, 44.64000000000000057, -5.000000000000000888 ) ) ;
#4664 = ORIENTED_EDGE ( 'NONE', *, *, #2051, .F. ) ;
#4665 = VERTEX_POINT ( 'NONE', #12412 ) ;
#4666 = ORIENTED_EDGE ( 'NONE', *, *, #5125, .T. ) ;
#4667 = CARTESIAN_POINT ( 'NONE',  ( 0.6666666666666951624, -4.233901974057275197, -3.300726591567086921 ) ) ;
#4668 = AXIS2_PLACEMENT_3D ( 'NONE', #12440, #5536, #3736 ) ;
#4669 = LINE ( 'NONE', #5573, #9988 ) ;
#4670 = DIRECTION ( 'NONE',  ( 0.000000000000000000, 0.000000000000000000, 1.000000000000000000 ) ) ;
#4671 = AXIS2_PLACEMENT_3D ( 'NONE', #8322, #10306, #1624 ) ;
#4672 = FACE_BOUND ( 'NONE', #4619, .T. ) ;
#4673 = EDGE_LOOP ( 'NONE', ( #12082, #119, #5321, #4753 ) ) ;
#4674 = CARTESIAN_POINT ( 'NONE',  ( 19.99999999999999645, 0.000000000000000000, 0.000000000000000000 ) ) ;
#4675 = ORIENTED_EDGE ( 'NONE', *, *, #7256, .F. ) ;
#4676 = VERTEX_POINT ( 'NONE', #8278 ) ;
#4677 = FACE_OUTER_BOUND ( 'NONE', #4693, .T. ) ;
#4678 = ORIENTED_EDGE ( 'NONE', *, *, #3547, .F. ) ;
#4679 = EDGE_LOOP ( 'NONE', ( #8303, #2911, #11582, #6243 ) ) ;
#4680 = SURFACE_STYLE_FILL_AREA ( #10335 ) ;
#4681 = AXIS2_PLACEMENT_3D ( 'NONE', #3853, #2842, #9622 ) ;
#4682 = EDGE_CURVE ( 'NONE', #11248, #7729, #5445, .T. ) ;
#4683 = EDGE_CURVE ( 'NONE', #5017, #9694, #8564, .T. ) ;
#4684 = DIRECTION ( 'NONE',  ( 1.000000000000000000, 0.000000000000000000, 0.000000000000000000 ) ) ;
#4685 = EDGE_CURVE ( 'NONE', #1261, #8686, #11378, .T. ) ;
#4686 = VERTEX_POINT ( 'NONE', #6482 ) ;
#4687 = DIRECTION ( 'NONE',  ( 0.000000000000000000, 1.530455820933490821E-32, -1.000000000000000000 ) ) ;
#4688 = CARTESIAN_POINT ( 'NONE',  ( 2.000000000000001776, -0.8865213383406761460, -1.535499999999995202 ) ) ;
#4689 = EDGE_LOOP ( 'NONE', ( #1797, #11902 ) ) ;
#4690 = PLANE ( 'NONE',  #6543 ) ;
#4691 = DIRECTION ( 'NONE',  ( -2.312964634635743450E-16, 0.9883022714608525883, -0.1525077710325583313 ) ) ;
#4692 = UNCERTAINTY_MEASURE_WITH_UNIT (LENGTH_MEASURE( 1.000000000000000082E-05 ), #10289, 'distance_accuracy_value', 'NONE');
#4693 = EDGE_LOOP ( 'NONE', ( #37, #3162, #3016, #7566 ) ) ;
#4694 = VERTEX_POINT ( 'NONE', #9479 ) ;
#4695 = FACE_OUTER_BOUND ( 'NONE', #7211, .T. ) ;
#4696 = DIRECTION ( 'NONE',  ( 1.942890293094023946E-16, 3.143117669239968912E-31, -1.000000000000000222 ) ) ;
#4697 = ORIENTED_EDGE ( 'NONE', *, *, #2205, .F. ) ;
#4698 = CARTESIAN_POINT ( 'NONE',  ( 0.000000000000000000, -4.707829255731254214, 5.709320773864518195 ) ) ;
#4699 = VECTOR ( 'NONE', #10070, 1000.000000000000000 ) ;
#4700 = LINE ( 'NONE', #6092, #9842 ) ;
#4701 = EDGE_CURVE ( 'NONE', #5907, #1263, #674, .T. ) ;
#4702 = DIRECTION ( 'NONE',  ( 0.000000000000000000, -1.530455820933490821E-32, 1.000000000000000000 ) ) ;
#4703 = CYLINDRICAL_SURFACE ( 'NONE', #3299, 2.800000000000003819 ) ;
#4704 = ORIENTED_EDGE ( 'NONE', *, *, #5466, .F. ) ;
#4705 = CIRCLE ( 'NONE', #11918, 7.400000000000009237 ) ;
#4706 = LINE ( 'NONE', #12578, #6378 ) ;
#4707 = ORIENTED_EDGE ( 'NONE', *, *, #8716, .F. ) ;
#4708 = CYLINDRICAL_SURFACE ( 'NONE', #10730, 2.500000000000000444 ) ;
#4709 =( NAMED_UNIT ( * ) PLANE_ANGLE_UNIT ( ) SI_UNIT ( $, .RADIAN. ) );
#4710 = EDGE_CURVE ( 'NONE', #9185, #1182, #4611, .T. ) ;
#4711 = EDGE_CURVE ( 'NONE', #3793, #7844, #5511, .T. ) ;
#4712 = LINE ( 'NONE', #2800, #8017 ) ;
#4713 = AXIS2_PLACEMENT_3D ( 'NONE', #1418, #2338, #7102 ) ;
#4714 = AXIS2_PLACEMENT_3D ( 'NONE', #7018, #5329, #2382 ) ;
#4715 = PLANE ( 'NONE',  #9708 ) ;
#4716 = FACE_OUTER_BOUND ( 'NONE', #11379, .T. ) ;
#4717 = AXIS2_PLACEMENT_3D ( 'NONE', #353, #8209, #9999 ) ;
#4718 = DIRECTION ( 'NONE',  ( -1.000000000000000000, 1.010728034814421376E-30, 1.090846720500930387E-30 ) ) ;
#4719 = CARTESIAN_POINT ( 'NONE',  ( 0.000000000000000000, -4.046291478462235247, 5.186098161460289901 ) ) ;
#4720 = FACE_OUTER_BOUND ( 'NONE', #11764, .T. ) ;
#4721 = CARTESIAN_POINT ( 'NONE',  ( 2.000000000000007105, 3.464101615137750390, 6.938893903907228378E-15 ) ) ;
#4722 = DIRECTION ( 'NONE',  ( 0.000000000000000000, 0.000000000000000000, 1.000000000000000000 ) ) ;
#4723 = CIRCLE ( 'NONE', #9837, 2.800000000000002931 ) ;
#4724 = STYLED_ITEM ( 'NONE', ( #7435 ), #10152 ) ;
#4725 = CIRCLE ( 'NONE', #4525, 2.800000000000003819 ) ;
#4726 = DIRECTION ( 'NONE',  ( -1.000000000000000000, 1.010728034814421376E-30, 1.090846720500930387E-30 ) ) ;
#4727 = EDGE_LOOP ( 'NONE', ( #10466, #12619, #12733, #11650, #7834, #9442, #1723, #4042, #7966, #4648 ) ) ;
#4728 = EDGE_CURVE ( 'NONE', #9867, #1053, #8968, .T. ) ;
#4729 = AXIS2_PLACEMENT_3D ( 'NONE', #11567, #3769, #8401 ) ;
#4730 = ORIENTED_EDGE ( 'NONE', *, *, #997, .T. ) ;
#4731 = ORIENTED_EDGE ( 'NONE', *, *, #8172, .F. ) ;
#4732 = LINE ( 'NONE', #8659, #9928 ) ;
#4733 = CIRCLE ( 'NONE', #4314, 6.000000000000000000 ) ;
#4734 = DIRECTION ( 'NONE',  ( 1.000000000000000000, 5.916456789157576279E-31, 0.000000000000000000 ) ) ;
#4735 = DIRECTION ( 'NONE',  ( -1.000000000000000000, 0.000000000000000000, 0.000000000000000000 ) ) ;
#4736 = CIRCLE ( 'NONE', #6998, 2.200000000000001066 ) ;
#4737 = AXIS2_PLACEMENT_3D ( 'NONE', #7425, #11355, #9902 ) ;
#4738 = DIRECTION ( 'NONE',  ( 1.140150527077241873E-30, 0.000000000000000000, -1.000000000000000000 ) ) ;
#4739 = EDGE_LOOP ( 'NONE', ( #4953, #2895, #8457, #5258 ) ) ;
#4740 = ADVANCED_FACE ( 'NONE', ( #2430 ), #6342, .F. ) ;
#4741 = DIRECTION ( 'NONE',  ( 0.000000000000000000, 0.000000000000000000, 1.000000000000000000 ) ) ;
#4742 = DIRECTION ( 'NONE',  ( -1.000000000000000000, 1.010728034814421376E-30, 1.090846720500930387E-30 ) ) ;
#4743 = EDGE_LOOP ( 'NONE', ( #9923, #4756, #994, #2039 ) ) ;
#4744 = ORIENTED_EDGE ( 'NONE', *, *, #375, .F. ) ;
#4745 = CARTESIAN_POINT ( 'NONE',  ( -10.00000000000000178, 0.000000000000000000, 0.000000000000000000 ) ) ;
#4746 = ORIENTED_EDGE ( 'NONE', *, *, #5952, .F. ) ;
#4747 = MECHANICAL_DESIGN_GEOMETRIC_PRESENTATION_REPRESENTATION (  '', ( #11741 ), #5160 ) ;
#4748 = AXIS2_PLACEMENT_3D ( 'NONE', #7467, #4505, #5471 ) ;
#4749 = ORIENTED_EDGE ( 'NONE', *, *, #1695, .F. ) ;
#4750 = CIRCLE ( 'NONE', #7988, 2.800000000000002931 ) ;
#4751 = SURFACE_STYLE_USAGE ( .BOTH. , #1655 ) ;
#4752 = CARTESIAN_POINT ( 'NONE',  ( 2.000000000000001776, 0.8865213383406727043, 1.535499999999998755 ) ) ;
#4753 = ORIENTED_EDGE ( 'NONE', *, *, #12732, .T. ) ;
#4754 = CARTESIAN_POINT ( 'NONE',  ( 2.000000000000001776, 1.773042676681341856, -3.469446951953614189E-15 ) ) ;
#4755 = FACE_OUTER_BOUND ( 'NONE', #9257, .T. ) ;
#4756 = ORIENTED_EDGE ( 'NONE', *, *, #6834, .T. ) ;
#4757 = DIRECTION ( 'NONE',  ( -1.000000000000000000, 1.010728034814421376E-30, 1.090846720500930387E-30 ) ) ;
#4758 = DIRECTION ( 'NONE',  ( 0.000000000000000000, 0.000000000000000000, 1.000000000000000000 ) ) ;
#4759 = EDGE_CURVE ( 'NONE', #4162, #11649, #9779, .T. ) ;
#4760 = EDGE_CURVE ( 'NONE', #1393, #837, #12604, .T. ) ;
#4761 = VERTEX_POINT ( 'NONE', #1768 ) ;
#4762 = ORIENTED_EDGE ( 'NONE', *, *, #1245, .T. ) ;
#4763 = ORIENTED_EDGE ( 'NONE', *, *, #10989, .F. ) ;
#4764 = DIRECTION ( 'NONE',  ( -1.000000000000000000, 1.010728034814421376E-30, 1.090846720500930387E-30 ) ) ;
#4765 = CIRCLE ( 'NONE', #5370, 2.149999999999992362 ) ;
#4766 = EDGE_LOOP ( 'NONE', ( #2177, #3979, #10529 ) ) ;
#4767 = CARTESIAN_POINT ( 'NONE',  ( 33.00000000000000000, 21.47552320888931021, -7.222675303056225182 ) ) ;
#4768 = LINE ( 'NONE', #2173, #9612 ) ;
#4769 = LINE ( 'NONE', #11852, #12245 ) ;
#4770 = AXIS2_PLACEMENT_3D ( 'NONE', #4133, #7870, #7039 ) ;
#4771 = EDGE_CURVE ( 'NONE', #9801, #10601, #10835, .T. ) ;
#4772 = CARTESIAN_POINT ( 'NONE',  ( 40.00000000000000711, 22.56100271565320980, -6.249672610153679919 ) ) ;
#4773 = ORIENTED_EDGE ( 'NONE', *, *, #10875, .T. ) ;
#4774 = LINE ( 'NONE', #10499, #5551 ) ;
#4775 = VERTEX_POINT ( 'NONE', #7634 ) ;
#4776 = DIRECTION ( 'NONE',  ( 1.000000000000000000, 1.081682119347366197E-16, -6.938893903907228378E-17 ) ) ;
#4777 = DIRECTION ( 'NONE',  ( 0.000000000000000000, 6.839766848137126197E-14, -1.000000000000000000 ) ) ;
#4778 = AXIS2_PLACEMENT_3D ( 'NONE', #10093, #5277, #1475 ) ;
#4779 = CARTESIAN_POINT ( 'NONE',  ( 9.757359312880696578, 13.00000000000000000, -4.242640687119267895 ) ) ;
#4780 = DIRECTION ( 'NONE',  ( -1.000000000000000000, 1.010728034814421376E-30, 1.090846720500930387E-30 ) ) ;
#4781 = DIRECTION ( 'NONE',  ( 4.314083075427402837E-32, -0.7227948638273978821, 0.6910626489868579858 ) ) ;
#4782 = CARTESIAN_POINT ( 'NONE',  ( -7.557654583407860981E-15, -4.647091401871400684, -3.572172305156889660 ) ) ;
#4783 = DIRECTION ( 'NONE',  ( -1.000000000000000000, -1.081682119347366444E-16, 5.551115123125780237E-17 ) ) ;
#4784 = EDGE_CURVE ( 'NONE', #7388, #10795, #3442, .T. ) ;
#4785 = DIRECTION ( 'NONE',  ( -1.000000000000000000, 1.010728034814421376E-30, 1.090846720500930387E-30 ) ) ;
#4786 = CIRCLE ( 'NONE', #6022, 2.149999999999985256 ) ;
#4787 = EDGE_CURVE ( 'NONE', #11478, #10207, #12488, .T. ) ;
#4788 = UNCERTAINTY_MEASURE_WITH_UNIT (LENGTH_MEASURE( 1.000000000000000082E-05 ), #10955, 'distance_accuracy_value', 'NONE');
#4789 = DIRECTION ( 'NONE',  ( 0.000000000000000000, -0.9989930665413151445, 0.04486483035050449486 ) ) ;
#4790 = EDGE_CURVE ( 'NONE', #11957, #9234, #12065, .T. ) ;
#4791 = CIRCLE ( 'NONE', #12622, 7.400000000000011902 ) ;
#4792 = ORIENTED_EDGE ( 'NONE', *, *, #268, .T. ) ;
#4793 = VERTEX_POINT ( 'NONE', #11686 ) ;
#4794 = AXIS2_PLACEMENT_3D ( 'NONE', #11149, #3248, #9009 ) ;
#4795 = DIRECTION ( 'NONE',  ( -1.000000000000000000, 1.010728034814421376E-30, 1.090846720500930387E-30 ) ) ;
#4796 = CIRCLE ( 'NONE', #884, 10.00000000000002309 ) ;
#4797 = CARTESIAN_POINT ( 'NONE',  ( 19.99999999999999645, 0.000000000000000000, 0.000000000000000000 ) ) ;
#4798 = DIRECTION ( 'NONE',  ( 0.000000000000000000, -1.000000000000000000, 0.000000000000000000 ) ) ;
#4799 = DIRECTION ( 'NONE',  ( -1.000000000000000000, 1.010728034814421376E-30, 1.090846720500930387E-30 ) ) ;
#4800 = ORIENTED_EDGE ( 'NONE', *, *, #11315, .T. ) ;
#4801 = DIRECTION ( 'NONE',  ( -1.000000000000000000, 0.000000000000000000, 0.000000000000000000 ) ) ;
#4802 = CYLINDRICAL_SURFACE ( 'NONE', #5355, 2.800000000000003819 ) ;
#4803 = ORIENTED_EDGE ( 'NONE', *, *, #7731, .F. ) ;
#4804 = AXIS2_PLACEMENT_3D ( 'NONE', #12219, #2427, #4854 ) ;
#4805 = ORIENTED_EDGE ( 'NONE', *, *, #5727, .F. ) ;
#4806 = CARTESIAN_POINT ( 'NONE',  ( 27.00000000000000355, 39.34792583643765340, -17.06347054209567560 ) ) ;
#4807 = EDGE_LOOP ( 'NONE', ( #8805, #7328, #5014, #8475 ) ) ;
#4808 = VERTEX_POINT ( 'NONE', #11569 ) ;
#4809 = CARTESIAN_POINT ( 'NONE',  ( 0.000000000000000000, 0.2110513566293374665, 7.396989747516548697 ) ) ;
#4810 = EDGE_LOOP ( 'NONE', ( #791, #5026, #1647, #3134 ) ) ;
#4811 = DIRECTION ( 'NONE',  ( 0.000000000000000000, 0.000000000000000000, 1.000000000000000000 ) ) ;
#4812 = DIRECTION ( 'NONE',  ( -1.000000000000000000, 1.010728034814421376E-30, 1.090846720500930387E-30 ) ) ;
#4813 = ORIENTED_EDGE ( 'NONE', *, *, #8251, .F. ) ;
#4814 = CIRCLE ( 'NONE', #10984, 4.000000000000001776 ) ;
#4815 = CARTESIAN_POINT ( 'NONE',  ( 40.00000000000000711, 16.67945018363952414, -6.690790236289299919 ) ) ;
#4816 = CARTESIAN_POINT ( 'NONE',  ( 19.99999999999999645, 3.565124043461683101, 5.527927226701645935 ) ) ;
#4817 = AXIS2_PLACEMENT_3D ( 'NONE', #6600, #1692, #11363 ) ;
#4818 = ORIENTED_EDGE ( 'NONE', *, *, #11619, .F. ) ;
#4819 = ORIENTED_EDGE ( 'NONE', *, *, #9496, .T. ) ;
#4820 = AXIS2_PLACEMENT_3D ( 'NONE', #12682, #1783, #2777 ) ;
#4821 = ORIENTED_EDGE ( 'NONE', *, *, #7689, .T. ) ;
#4822 = DIRECTION ( 'NONE',  ( 1.000000000000000000, 0.000000000000000000, 0.000000000000000000 ) ) ;
#4823 = ORIENTED_EDGE ( 'NONE', *, *, #1451, .T. ) ;
#4824 = ADVANCED_FACE ( 'NONE', ( #4672, #8724, #795 ), #7876, .F. ) ;
#4825 = CARTESIAN_POINT ( 'NONE',  ( 2.000000000000001776, 1.773042676681338303, 0.000000000000000000 ) ) ;
#4826 = ORIENTED_EDGE ( 'NONE', *, *, #6419, .T. ) ;
#4827 = VECTOR ( 'NONE', #5285, 1000.000000000000000 ) ;
#4828 = AXIS2_PLACEMENT_3D ( 'NONE', #7278, #4370, #11200 ) ;
#4829 = CARTESIAN_POINT ( 'NONE',  ( 19.99999999999997868, -2.385831757338501724, -6.045230171438906730 ) ) ;
#4830 = LINE ( 'NONE', #2923, #11424 ) ;
#4831 = DIRECTION ( 'NONE',  ( 1.000000000000000000, -1.010728034814421376E-30, -1.090846720500930387E-30 ) ) ;
#4832 = ORIENTED_EDGE ( 'NONE', *, *, #5499, .F. ) ;
#4833 = DIRECTION ( 'NONE',  ( -1.000000000000000000, 1.010728034814421376E-30, 1.090846720500930387E-30 ) ) ;
#4834 = AXIS2_PLACEMENT_3D ( 'NONE', #6113, #10021, #11069 ) ;
#4835 = VERTEX_POINT ( 'NONE', #1953 ) ;
#4836 = AXIS2_PLACEMENT_3D ( 'NONE', #7068, #6096, #946 ) ;
#4837 = DIRECTION ( 'NONE',  ( 1.000000000000000000, 0.000000000000000000, 0.000000000000000000 ) ) ;
#4838 = EDGE_CURVE ( 'NONE', #10019, #1763, #7695, .T. ) ;
#4839 = LINE ( 'NONE', #1933, #9649 ) ;
#4840 = EDGE_CURVE ( 'NONE', #8271, #3837, #6862, .T. ) ;
#4841 = FACE_OUTER_BOUND ( 'NONE', #7408, .T. ) ;
#4842 = CARTESIAN_POINT ( 'NONE',  ( 19.99999999999997868, 6.544726022087268724, -0.6592800351836389794 ) ) ;
#4843 = DIRECTION ( 'NONE',  ( -5.208075316782971161E-17, -0.1525077710325583313, -0.9883022714608525883 ) ) ;
#4844 = AXIS2_PLACEMENT_3D ( 'NONE', #9985, #6139, #469 ) ;
#4845 = CARTESIAN_POINT ( 'NONE',  ( 0.000000000000000000, 1.531833341630221224, -6.396997380212695816 ) ) ;
#4846 = DIRECTION ( 'NONE',  ( -1.000000000000000000, 1.010728034814421376E-30, 1.090846720500930387E-30 ) ) ;
#4847 = CARTESIAN_POINT ( 'NONE',  ( -2.099999999999965450, -3.212271124132670141E-15, -5.000000000000011546 ) ) ;
#4848 = CARTESIAN_POINT ( 'NONE',  ( 20.00000000000000000, 15.24625277455639072, -6.248133273622503481 ) ) ;
#4849 = VECTOR ( 'NONE', #4584, 1000.000000000000000 ) ;
#4850 = ADVANCED_FACE ( 'NONE', ( #4857 ), #5757, .F. ) ;
#4851 =( REPRESENTATION_RELATIONSHIP ('NONE','NONE', #10018, #9199 ) REPRESENTATION_RELATIONSHIP_WITH_TRANSFORMATION ( #8205 )SHAPE_REPRESENTATION_RELATIONSHIP( ) );
#4852 = ORIENTED_EDGE ( 'NONE', *, *, #2480, .T. ) ;
#4853 = ORIENTED_EDGE ( 'NONE', *, *, #852, .T. ) ;
#4854 = DIRECTION ( 'NONE',  ( 1.000000000000000000, 5.916456789157576279E-31, 0.000000000000000000 ) ) ;
#4855 = LINE ( 'NONE', #9729, #2204 ) ;
#4856 = FACE_OUTER_BOUND ( 'NONE', #11883, .T. ) ;
#4857 = FACE_OUTER_BOUND ( 'NONE', #5580, .T. ) ;
#4858 = ORIENTED_EDGE ( 'NONE', *, *, #11792, .F. ) ;
#4859 = DIRECTION ( 'NONE',  ( 0.000000000000000000, 0.000000000000000000, -1.000000000000000000 ) ) ;
#4860 = DIRECTION ( 'NONE',  ( 0.000000000000000000, 1.467581828789149532E-15, 1.000000000000000000 ) ) ;
#4861 = EDGE_CURVE ( 'NONE', #9789, #477, #11862, .T. ) ;
#4862 = VECTOR ( 'NONE', #7231, 1000.000000000000000 ) ;
#4863 = LINE ( 'NONE', #12730, #7831 ) ;
#4864 = EDGE_LOOP ( 'NONE', ( #620, #12229, #7498, #4623 ) ) ;
#4865 = B_SPLINE_CURVE_WITH_KNOTS ( 'NONE', 3,
 ( #4527, #1616, #11485, #6458, #2667 ),
 .UNSPECIFIED., .F., .F.,
 ( 4, 1, 4 ),
 ( 0.000000000000000000, 0.002309401076758506657, 0.004618802153517013315 ),
 .UNSPECIFIED. ) ;
#4866 = ORIENTED_EDGE ( 'NONE', *, *, #3972, .F. ) ;
#4867 = CARTESIAN_POINT ( 'NONE',  ( 19.99999999999999645, 0.000000000000000000, 0.000000000000000000 ) ) ;
#4868 = ORIENTED_EDGE ( 'NONE', *, *, #1847, .T. ) ;
#4869 = ORIENTED_EDGE ( 'NONE', *, *, #6913, .T. ) ;
#4870 = DIRECTION ( 'NONE',  ( 0.000000000000000000, 0.000000000000000000, 1.000000000000000000 ) ) ;
#4871 = CARTESIAN_POINT ( 'NONE',  ( 3.469446951953614189E-14, -3.469446951953614189E-15, -5.000000000000011546 ) ) ;
#4872 = ORIENTED_EDGE ( 'NONE', *, *, #3957, .F. ) ;
#4873 = AXIS2_PLACEMENT_3D ( 'NONE', #3508, #535, #4400 ) ;
#4874 = ADVANCED_FACE ( 'NONE', ( #10706 ), #10768, .F. ) ;
#4875 = CARTESIAN_POINT ( 'NONE',  ( 19.99999999999997868, 0.3649881613860929686, -6.567714405409704526 ) ) ;
#4876 = AXIS2_PLACEMENT_3D ( 'NONE', #4349, #9229, #8276 ) ;
#4877 = EDGE_CURVE ( 'NONE', #3242, #9347, #2883, .T. ) ;
#4878 = DIRECTION ( 'NONE',  ( -1.000000000000000000, 1.010728034814421376E-30, 1.090846720500930387E-30 ) ) ;
#4879 = ORIENTED_EDGE ( 'NONE', *, *, #964, .T. ) ;
#4880 = DIRECTION ( 'NONE',  ( -1.000000000000000000, -1.031065855027150586E-29, 2.218671295934095703E-30 ) ) ;
#4881 = PRODUCT_DEFINITION_CONTEXT ( 'detailed design', #826, 'design' ) ;
#4882 = CARTESIAN_POINT ( 'NONE',  ( 20.00000000000000355, 14.39651704831740808, -19.59866274153860388 ) ) ;
#4883 = AXIS2_PLACEMENT_3D ( 'NONE', #10057, #7880, #2225 ) ;
#4884 = CONICAL_SURFACE ( 'NONE', #7150, 1.535500000000001863, 1.047197551196590748 ) ;
#4885 = VERTEX_POINT ( 'NONE', #8841 ) ;
#4886 = VECTOR ( 'NONE', #9091, 1000.000000000000000 ) ;
#4887 = ORIENTED_EDGE ( 'NONE', *, *, #3659, .T. ) ;
#4888 = VERTEX_POINT ( 'NONE', #5819 ) ;
#4889 = PLANE ( 'NONE',  #3768 ) ;
#4890 = ORIENTED_EDGE ( 'NONE', *, *, #896, .T. ) ;
#4891 = CARTESIAN_POINT ( 'NONE',  ( 2.345747346278117096, -3.264484291692501206, -0.01223254789874552578 ) ) ;
#4892 = VERTEX_POINT ( 'NONE', #12536 ) ;
#4893 = VECTOR ( 'NONE', #168, 1000.000000000000000 ) ;
#4894 = EDGE_CURVE ( 'NONE', #8701, #9489, #5683, .T. ) ;
#4895 = EDGE_CURVE ( 'NONE', #9520, #8041, #5479, .T. ) ;
#4896 = DIRECTION ( 'NONE',  ( -1.000000000000000000, 1.010728034814421376E-30, 1.090846720500930387E-30 ) ) ;
#4897 = CARTESIAN_POINT ( 'NONE',  ( 0.000000000000000000, -4.618802153517027165, -5.000000000000000888 ) ) ;
#4898 = ORIENTED_EDGE ( 'NONE', *, *, #10360, .F. ) ;
#4899 = CARTESIAN_POINT ( 'NONE',  ( 20.00000000000000355, 21.47552320888931021, -7.222675303056224294 ) ) ;
#4900 = ORIENTED_EDGE ( 'NONE', *, *, #217, .T. ) ;
#4901 = LINE ( 'NONE', #7859, #11364 ) ;
#4902 = CARTESIAN_POINT ( 'NONE',  ( 19.99999999999997868, 1.834336845376804748, -6.234758161925229913 ) ) ;
#4903 = ADVANCED_FACE ( 'NONE', ( #5944 ), #3240, .F. ) ;
#4904 = DIRECTION ( 'NONE',  ( 0.000000000000000000, 5.551115123125776539E-17, 1.000000000000000000 ) ) ;
#4905 = CARTESIAN_POINT ( 'NONE',  ( 0.000000000000000000, -2.385831757338585657, 6.045230171438855216 ) ) ;
#4906 = CYLINDRICAL_SURFACE ( 'NONE', #5488, 2.800000000000003819 ) ;
#4907 = CARTESIAN_POINT ( 'NONE',  ( 0.000000000000000000, 0.8865213383406657099, 1.535500000000022958 ) ) ;
#4908 = VECTOR ( 'NONE', #12347, 1000.000000000000000 ) ;
#4909 = DIRECTION ( 'NONE',  ( -1.000000000000000000, 1.010728034814421376E-30, 1.090846720500930387E-30 ) ) ;
#4910 = EDGE_CURVE ( 'NONE', #6552, #4118, #9575, .T. ) ;
#4911 = B_SPLINE_CURVE_WITH_KNOTS ( 'NONE', 3,
 ( #2467, #5354, #5417, #7422, #9271 ),
 .UNSPECIFIED., .F., .F.,
 ( 4, 1, 4 ),
 ( 0.000000000000000000, 0.002309401076758506657, 0.004618802153517013315 ),
 .UNSPECIFIED. ) ;
#4912 = CARTESIAN_POINT ( 'NONE',  ( 19.99999999999999645, 5.914787828628542243, 4.446941076999763709 ) ) ;
#4913 = ADVANCED_FACE ( 'NONE', ( #7112 ), #4142, .T. ) ;
#4914 = EDGE_CURVE ( 'NONE', #9071, #9362, #130, .T. ) ;
#4915 = CARTESIAN_POINT ( 'NONE',  ( 14.00000000000000000, 30.00000000000000000, 0.000000000000000000 ) ) ;
#4916 = EDGE_LOOP ( 'NONE', ( #9056, #4274, #12454, #8127 ) ) ;
#4917 = DIRECTION ( 'NONE',  ( 0.000000000000000000, 0.000000000000000000, 1.000000000000000000 ) ) ;
#4918 = CARTESIAN_POINT ( 'NONE',  ( 2.000000000000001776, 0.8865213383406622683, -1.535499999999995202 ) ) ;
#4919 = CARTESIAN_POINT ( 'NONE',  ( 19.99999999999997868, 0.2110513566294510979, -7.396989747516558467 ) ) ;
#4920 = FACE_OUTER_BOUND ( 'NONE', #10327, .T. ) ;
#4921 = CARTESIAN_POINT ( 'NONE',  ( 11.00000000000003375, -6.123233995736749519E-16, 20.00000000000003553 ) ) ;
#4922 = EDGE_LOOP ( 'NONE', ( #6338, #11445, #2976, #10317 ) ) ;
#4923 = DIRECTION ( 'NONE',  ( -1.000000000000000000, 1.010728034814421376E-30, 1.090846720500930387E-30 ) ) ;
#4924 = VECTOR ( 'NONE', #6972, 1000.000000000000000 ) ;
#4925 = CIRCLE ( 'NONE', #10471, 6.499000000000008548 ) ;
#4926 = DIRECTION ( 'NONE',  ( 1.000000000000000000, 1.031065855027150586E-29, -2.218671295934095703E-30 ) ) ;
#4927 = FACE_OUTER_BOUND ( 'NONE', #8500, .T. ) ;
#4928 = EDGE_LOOP ( 'NONE', ( #12326, #2688 ) ) ;
#4929 = CIRCLE ( 'NONE', #8601, 2.149999999999988809 ) ;
#4930 = ORIENTED_EDGE ( 'NONE', *, *, #8076, .T. ) ;
#4931 = LINE ( 'NONE', #8851, #3125 ) ;
#4932 = ORIENTED_EDGE ( 'NONE', *, *, #5025, .F. ) ;
#4933 = VERTEX_POINT ( 'NONE', #149 ) ;
#4934 =( NAMED_UNIT ( * ) SI_UNIT ( $, .STERADIAN. ) SOLID_ANGLE_UNIT ( ) );
#4935 = LINE ( 'NONE', #3081, #12145 ) ;
#4936 = VECTOR ( 'NONE', #9005, 1000.000000000000000 ) ;
#4937 = VERTEX_POINT ( 'NONE', #6073 ) ;
#4938 = VECTOR ( 'NONE', #2898, 1000.000000000000000 ) ;
#4939 = CARTESIAN_POINT ( 'NONE',  ( -40.00000000000000000, 19.99999999999999645, 2.000000000000003109 ) ) ;
#4940 = EDGE_CURVE ( 'NONE', #3717, #3737, #7132, .T. ) ;
#4941 = FACE_OUTER_BOUND ( 'NONE', #6769, .T. ) ;
#4942 = EDGE_CURVE ( 'NONE', #7374, #3414, #86, .T. ) ;
#4943 = ORIENTED_EDGE ( 'NONE', *, *, #4957, .F. ) ;
#4944 = CARTESIAN_POINT ( 'NONE',  ( 9.000000000000035527, -19.99999999999999645, 14.15000000000002878 ) ) ;
#4945 = CYLINDRICAL_SURFACE ( 'NONE', #2798, 7.400000000000010125 ) ;
#4946 = AXIS2_PLACEMENT_3D ( 'NONE', #10284, #8486, #4374 ) ;
#4947 = VECTOR ( 'NONE', #3991, 1000.000000000000114 ) ;
#4948 = VECTOR ( 'NONE', #12642, 999.9999999999998863 ) ;
#4949 = ADVANCED_FACE ( 'NONE', ( #10113 ), #1566, .T. ) ;
#4950 = VERTEX_POINT ( 'NONE', #9861 ) ;
#4951 = VERTEX_POINT ( 'NONE', #1302 ) ;
#4952 = EDGE_CURVE ( 'NONE', #6148, #11828, #6101, .T. ) ;
#4953 = ORIENTED_EDGE ( 'NONE', *, *, #10787, .T. ) ;
#4954 = EDGE_CURVE ( 'NONE', #2575, #3892, #1168, .T. ) ;
#4955 = DIRECTION ( 'NONE',  ( 0.000000000000000000, 0.000000000000000000, -1.000000000000000000 ) ) ;
#4956 = ORIENTED_EDGE ( 'NONE', *, *, #3275, .F. ) ;
#4957 = EDGE_CURVE ( 'NONE', #8459, #3414, #8980, .T. ) ;
#4958 = DIRECTION ( 'NONE',  ( 1.000000000000000000, -6.162975822039154730E-33, -4.563833282352349791E-17 ) ) ;
#4959 = MECHANICAL_DESIGN_GEOMETRIC_PRESENTATION_REPRESENTATION (  '', ( #12372 ), #10279 ) ;
#4960 = ORIENTED_EDGE ( 'NONE', *, *, #10619, .T. ) ;
#4961 = DIRECTION ( 'NONE',  ( 0.000000000000000000, 0.000000000000000000, -1.000000000000000000 ) ) ;
#4962 = DIRECTION ( 'NONE',  ( -1.000000000000000000, 0.000000000000000000, 0.000000000000000000 ) ) ;
#4963 = VERTEX_POINT ( 'NONE', #3198 ) ;
#4965 = LINE ( 'NONE', #8880, #4947 ) ;
#4964 = STYLED_ITEM ( 'NONE', ( #10686 ), #1739 ) ;
#4966 = ORIENTED_EDGE ( 'NONE', *, *, #1451, .F. ) ;
#4967 = CARTESIAN_POINT ( 'NONE',  ( 19.99999999999999645, 0.000000000000000000, 0.000000000000000000 ) ) ;
#4968 =( NAMED_UNIT ( * ) PLANE_ANGLE_UNIT ( ) SI_UNIT ( $, .RADIAN. ) );
#4969 = EDGE_CURVE ( 'NONE', #5919, #9871, #3857, .T. ) ;
#4970 = DIRECTION ( 'NONE',  ( 9.367723249499501176E-31, -0.9989930665413151445, 0.04486483035050449486 ) ) ;
#4971 = CARTESIAN_POINT ( 'NONE',  ( 3.469446951953614189E-14, -3.469446951953614189E-15, -5.000000000000011546 ) ) ;
#4972 = LINE ( 'NONE', #12647, #6537 ) ;
#4973 = CARTESIAN_POINT ( 'NONE',  ( -3.349226789952653327, -2.685125164760732375, -0.2236248678334778750 ) ) ;
#4974 = DIRECTION ( 'NONE',  ( 4.703787633549127174E-18, 0.9883022714608525883, -0.1525077710325581370 ) ) ;
#4975 = CARTESIAN_POINT ( 'NONE',  ( 33.00000000000001421, 39.34792583643766761, -10.06347054209568270 ) ) ;
#4976 = CARTESIAN_POINT ( 'NONE',  ( 19.99999999999997868, 5.483475578891663815, -3.488337222187519515 ) ) ;
#4977 = DIRECTION ( 'NONE',  ( 0.000000000000000000, 0.000000000000000000, 1.000000000000000000 ) ) ;
#4978 = ORIENTED_EDGE ( 'NONE', *, *, #6766, .T. ) ;
#4979 = ORIENTED_EDGE ( 'NONE', *, *, #11606, .F. ) ;
#4980 = EDGE_CURVE ( 'NONE', #349, #11641, #6137, .T. ) ;
#4981 = DIRECTION ( 'NONE',  ( 0.000000000000000000, -1.530455820933490821E-32, 1.000000000000000000 ) ) ;
#4982 = CYLINDRICAL_SURFACE ( 'NONE', #9376, 6.499000000000010324 ) ;
#4984 = EDGE_CURVE ( 'NONE', #9732, #3763, #4985, .T. ) ;
#4983 = LINE ( 'NONE', #2881, #9822 ) ;
#4985 = LINE ( 'NONE', #1240, #10200 ) ;
#4986 = ORIENTED_EDGE ( 'NONE', *, *, #1422, .F. ) ;
#4987 = CARTESIAN_POINT ( 'NONE',  ( 8.000000000000000000, 30.00000000000000000, -7.347880794884119736E-16 ) ) ;
#4988 = AXIS2_PLACEMENT_3D ( 'NONE', #10624, #11666, #776 ) ;
#4989 = DIRECTION ( 'NONE',  ( 1.000000000000000000, 0.000000000000000000, 0.000000000000000000 ) ) ;
#4990 = DIRECTION ( 'NONE',  ( 7.038118388768704892E-30, 0.4999999999999992784, -0.8660254037844390407 ) ) ;
#4991 = EDGE_LOOP ( 'NONE', ( #83, #12550, #3027, #8078, #3269, #1634, #3781, #2539, #9178 ) ) ;
#4992 = ORIENTED_EDGE ( 'NONE', *, *, #11792, .T. ) ;
#4993 = FACE_OUTER_BOUND ( 'NONE', #11562, .T. ) ;
#4994 = VERTEX_POINT ( 'NONE', #5237 ) ;
#4995 = ORIENTED_EDGE ( 'NONE', *, *, #9015, .T. ) ;
#4996 = DIRECTION ( 'NONE',  ( 1.000000000000000000, 0.000000000000000000, 0.000000000000000000 ) ) ;
#4997 = CLOSED_SHELL ( 'NONE', ( #3021, #11005, #6157, #1816, #9265, #2972, #6415, #909, #11158, #6269, #10783, #9884, #12340, #4397, #1234, #432, #6352, #5176, #8655, #9938, #3314, #1997, #1802, #2764, #9967, #2813, #6792, #3895, #2753, #11336, #3770, #10025, #12592, #7516, #10204, #1684, #11047, #4562, #6249, #11998, #8504, #2525, #9148, #2452, #12069, #9451, #9227, #6813, #5730, #3416, #9301, #7304, #2102, #12383, #11, #1448, #3165, #11590, #7777, #1519, #1211, #504, #6389, #6442, #3982, #6493, #184, #7238, #7080, #3231, #4158, #1059, #3224, #2114, #7929, #4637, #4233, #9529, #12273, #8843, #3308, #12121, #11769, #11044, #9950, #6230, #2708, #3723, #4391, #10606, #9725, #7995, #6010, #11211, #4124, #2459, #4034, #462, #7146, #513, #5253, #11744, #3034, #1084, #2589, #2649, #10804, #5390, #9798, #5482, #3687, #2116, #5015, #8091, #27, #10489, #4913, #8487, #10796, #3204, #8207, #12681, #11167, #10283, #7015, #8043, #1771, #732, #7149, #6695, #6676, #2243, #2221, #2922, #7393, #1939, #3761, #109, #10911, #6120, #8485, #10826, #4064, #12113, #1726, #2320, #7126, #9564 ) ) ;
#4998 = VECTOR ( 'NONE', #114, 1000.000000000000000 ) ;
#4999 = CYLINDRICAL_SURFACE ( 'NONE', #9030, 2.800000000000003819 ) ;
#5000 = ORIENTED_EDGE ( 'NONE', *, *, #5663, .T. ) ;
#5001 = CARTESIAN_POINT ( 'NONE',  ( 2.000000000000001776, -0.8865213383406727043, 1.535500000000009191 ) ) ;
#5002 = CARTESIAN_POINT ( 'NONE',  ( 19.99999999999999645, 0.000000000000000000, 0.000000000000000000 ) ) ;
#5003 = EDGE_CURVE ( 'NONE', #6740, #3160, #12295, .T. ) ;
#5004 = ORIENTED_EDGE ( 'NONE', *, *, #2224, .T. ) ;
#5005 = CARTESIAN_POINT ( 'NONE',  ( 0.000000000000000000, 12.99999999999999822, 0.000000000000000000 ) ) ;
#5006 = LINE ( 'NONE', #105, #3618 ) ;
#5007 = B_SPLINE_CURVE_WITH_KNOTS ( 'NONE', 3,
 ( #599, #9346, #11237, #6271, #6333, #6403 ),
 .UNSPECIFIED., .F., .F.,
 ( 4, 2, 4 ),
 ( -3.640115492410384041E-06, 0.0002066546034003272525, 0.0004169493222930648578 ),
 .UNSPECIFIED. ) ;
#5008 = EDGE_LOOP ( 'NONE', ( #12342, #3886, #919, #8081 ) ) ;
#5009 = EDGE_LOOP ( 'NONE', ( #5851, #9289, #10683, #2178 ) ) ;
#5010 = ORIENTED_EDGE ( 'NONE', *, *, #9031, .F. ) ;
#5011 = DIRECTION ( 'NONE',  ( -0.000000000000000000, -0.000000000000000000, -1.000000000000000000 ) ) ;
#5012 = VECTOR ( 'NONE', #9339, 1000.000000000000000 ) ;
#5013 = CARTESIAN_POINT ( 'NONE',  ( 0.1410422978106194436, -4.700232962125120650, -3.687027686973640694 ) ) ;
#5014 = ORIENTED_EDGE ( 'NONE', *, *, #1683, .T. ) ;
#5015 = ADVANCED_FACE ( 'NONE', ( #11098 ), #275, .T. ) ;
#5016 = PLANE ( 'NONE',  #5327 ) ;
#5017 = VERTEX_POINT ( 'NONE', #339 ) ;
#5018 = EDGE_CURVE ( 'NONE', #11532, #12678, #4269, .T. ) ;
#5019 = DIRECTION ( 'NONE',  ( 1.000000000000000000, 1.081682119347366321E-16, -6.938893903907228378E-17 ) ) ;
#5020 = EDGE_CURVE ( 'NONE', #2782, #6170, #11463, .T. ) ;
#5021 = CARTESIAN_POINT ( 'NONE',  ( 2.807080416178990845, -3.225969019225313872, -3.502507215260560969 ) ) ;
#5022 = AXIS2_PLACEMENT_3D ( 'NONE', #11610, #2803, #1811 ) ;
#5023 = FACE_OUTER_BOUND ( 'NONE', #1650, .T. ) ;
#5024 = APPLICATION_CONTEXT ( 'automotive_design' ) ;
#5025 = EDGE_CURVE ( 'NONE', #8204, #2582, #2350, .T. ) ;
#5026 = ORIENTED_EDGE ( 'NONE', *, *, #11372, .T. ) ;
#5027 = DIRECTION ( 'NONE',  ( 0.000000000000000000, 0.000000000000000000, 1.000000000000000000 ) ) ;
#5028 = ORIENTED_EDGE ( 'NONE', *, *, #3926, .T. ) ;
#5029 = DIRECTION ( 'NONE',  ( 0.000000000000000000, 0.5000000000000011102, 0.8660254037844379305 ) ) ;
#5030 = PRESENTATION_STYLE_ASSIGNMENT (( #10030 ) ) ;
#5031 = CIRCLE ( 'NONE', #9944, 2.149999999999985256 ) ;
#5032 = LINE ( 'NONE', #129, #2054 ) ;
#5033 = DIRECTION ( 'NONE',  ( 0.000000000000000000, 0.000000000000000000, 1.000000000000000000 ) ) ;
#5034 = EDGE_CURVE ( 'NONE', #5244, #11248, #7305, .T. ) ;
#5035 = DIRECTION ( 'NONE',  ( -0.3420201433256680468, -7.946868433027814422E-32, 0.9396926207859086499 ) ) ;
#5036 = DIRECTION ( 'NONE',  ( -1.000000000000000000, -1.031065855027150586E-29, 2.218671295934095703E-30 ) ) ;
#5037 = DIRECTION ( 'NONE',  ( 0.000000000000000000, 0.000000000000000000, -1.000000000000000000 ) ) ;
#5038 = AXIS2_PLACEMENT_3D ( 'NONE', #8171, #1151, #9958 ) ;
#5039 = AXIS2_PLACEMENT_3D ( 'NONE', #8359, #9313, #8423 ) ;
#5040 = CARTESIAN_POINT ( 'NONE',  ( -11.83215956619923226, 30.00000000000000000, -4.336808689942017736E-16 ) ) ;
#5041 = CARTESIAN_POINT ( 'NONE',  ( 4.000000000000003553, 0.000000000000000000, 0.000000000000000000 ) ) ;
#5042 = CARTESIAN_POINT ( 'NONE',  ( 0.000000000000000000, -5.651611091574772594, -4.776954267060654402 ) ) ;
#5043 =( NAMED_UNIT ( * ) SI_UNIT ( $, .STERADIAN. ) SOLID_ANGLE_UNIT ( ) );
#5044 = CONICAL_SURFACE ( 'NONE', #1137, 4.000000000000000000, 0.8911886515913786111 ) ;
#5045 = ORIENTED_EDGE ( 'NONE', *, *, #3391, .F. ) ;
#5046 = VECTOR ( 'NONE', #10072, 1000.000000000000114 ) ;
#5047 = CARTESIAN_POINT ( 'NONE',  ( -17.00000000000000000, 2.531464386849852200E-30, 22.15000000000006608 ) ) ;
#5048 = CARTESIAN_POINT ( 'NONE',  ( 33.00000000000001421, 81.84122341717352356, -27.68198508464163510 ) ) ;
#5049 = FACE_OUTER_BOUND ( 'NONE', #7186, .T. ) ;
#5050 = CARTESIAN_POINT ( 'NONE',  ( 40.00000000000006395, 1.290960574571364216E-15, -20.00000000000000000 ) ) ;
#5051 = DIRECTION ( 'NONE',  ( 0.000000000000000000, 1.530455820933490821E-32, -1.000000000000000000 ) ) ;
#5052 = EDGE_LOOP ( 'NONE', ( #12492, #6427 ) ) ;
#5053 = ADVANCED_FACE ( 'NONE', ( #3449 ), #1562, .T. ) ;
#5054 = LINE ( 'NONE', #2885, #920 ) ;
#5055 = CARTESIAN_POINT ( 'NONE',  ( 27.00000000000001421, 39.34792583643766761, -10.06347054209568270 ) ) ;
#5056 = DIRECTION ( 'NONE',  ( -0.000000000000000000, -1.000000000000000000, -0.000000000000000000 ) ) ;
#5057 = VERTEX_POINT ( 'NONE', #3634 ) ;
#5058 = CIRCLE ( 'NONE', #6078, 0.2000000000000000944 ) ;
#5059 = EDGE_LOOP ( 'NONE', ( #3405, #12376 ) ) ;
#5060 = CARTESIAN_POINT ( 'NONE',  ( 19.99999999999999645, 0.000000000000000000, 0.000000000000000000 ) ) ;
#5061 = ORIENTED_EDGE ( 'NONE', *, *, #10966, .F. ) ;
#5062 = ORIENTED_EDGE ( 'NONE', *, *, #1913, .T. ) ;
#5063 = PRODUCT_CONTEXT ( 'NONE', #6331, 'mechanical' ) ;
#5064 = DIRECTION ( 'NONE',  ( 0.000000000000000000, 0.000000000000000000, -1.000000000000000000 ) ) ;
#5065 = ORIENTED_EDGE ( 'NONE', *, *, #5148, .F. ) ;
#5066 = LINE ( 'NONE', #11642, #3694 ) ;
#5067 = DIRECTION ( 'NONE',  ( -1.000000000000000000, 1.010728034814421376E-30, 1.090846720500930387E-30 ) ) ;
#5068 = VERTEX_POINT ( 'NONE', #12397 ) ;
#5069 = FACE_BOUND ( 'NONE', #12624, .T. ) ;
#5070 = CARTESIAN_POINT ( 'NONE',  ( 0.000000000000000000, 0.000000000000000000, 0.000000000000000000 ) ) ;
#5071 = AXIS2_PLACEMENT_3D ( 'NONE', #6952, #4041, #8230 ) ;
#5072 = DIRECTION ( 'NONE',  ( 0.000000000000000000, 0.000000000000000000, -1.000000000000000000 ) ) ;
#5073 = VERTEX_POINT ( 'NONE', #5559 ) ;
#5074 = VERTEX_POINT ( 'NONE', #2476 ) ;
#5075 = EDGE_CURVE ( 'NONE', #2162, #4279, #343, .T. ) ;
#5076 = ORIENTED_EDGE ( 'NONE', *, *, #4942, .T. ) ;
#5077 = EDGE_CURVE ( 'NONE', #12721, #222, #5866, .T. ) ;
#5078 = ADVANCED_FACE ( 'NONE', ( #6464 ), #1431, .F. ) ;
#5079 = VERTEX_POINT ( 'NONE', #7489 ) ;
#5080 = AXIS2_PLACEMENT_3D ( 'NONE', #2014, #12664, #3831 ) ;
#5081 = DIRECTION ( 'NONE',  ( 1.000000000000000000, -1.010728034814421376E-30, -1.090846720500930387E-30 ) ) ;
#5082 = DIRECTION ( 'NONE',  ( -1.000000000000000000, 1.010728034814421376E-30, 1.090846720500930387E-30 ) ) ;
#5083 = VERTEX_POINT ( 'NONE', #12206 ) ;
#5084 = CARTESIAN_POINT ( 'NONE',  ( 40.00000000000000711, 11.34118543499637255, -24.03007857557328464 ) ) ;
#5085 = ORIENTED_EDGE ( 'NONE', *, *, #2334, .F. ) ;
#5086 = CARTESIAN_POINT ( 'NONE',  ( 19.99999999999999645, 3.681899619563770543, 5.450844343808956438 ) ) ;
#5087 = AXIS2_PLACEMENT_3D ( 'NONE', #1936, #12520, #7616 ) ;
#5088 = AXIS2_PLACEMENT_3D ( 'NONE', #4842, #8886, #8768 ) ;
#5089 = DIRECTION ( 'NONE',  ( -1.140150527077241873E-30, 0.000000000000000000, 1.000000000000000000 ) ) ;
#5090 = DIRECTION ( 'NONE',  ( 1.000000000000000000, -1.010728034814421376E-30, -1.090846720500930387E-30 ) ) ;
#5091 = ORIENTED_EDGE ( 'NONE', *, *, #3112, .T. ) ;
#5092 = CARTESIAN_POINT ( 'NONE',  ( 19.99999999999999645, -6.182645281642508372, 2.245659411033100294 ) ) ;
#5093 = ORIENTED_EDGE ( 'NONE', *, *, #6520, .T. ) ;
#5094 = FACE_OUTER_BOUND ( 'NONE', #5760, .T. ) ;
#5095 = CONICAL_SURFACE ( 'NONE', #2643, 1.610000000000001874, 0.7853981633974658205 ) ;
#5096 = CARTESIAN_POINT ( 'NONE',  ( 19.99999999999999645, -3.178467454237171363, 5.758943784352557493 ) ) ;
#5097 = CARTESIAN_POINT ( 'NONE',  ( 40.00000000000000711, 14.50364731389636574, -24.59751492040896892 ) ) ;
#5098 = ADVANCED_FACE ( 'NONE', ( #11426 ), #10442, .T. ) ;
#5099 = FACE_OUTER_BOUND ( 'NONE', #1343, .T. ) ;
#5100 = LINE ( 'NONE', #4130, #11209 ) ;
#5101 = CARTESIAN_POINT ( 'NONE',  ( 0.000000000000000000, -5.610543508060457540, 3.433640984893238102 ) ) ;
#5102 = DIRECTION ( 'NONE',  ( 0.000000000000000000, -1.000000000000000000, 0.000000000000000000 ) ) ;
#5103 = EDGE_CURVE ( 'NONE', #9103, #10993, #5298, .T. ) ;
#5104 = CARTESIAN_POINT ( 'NONE',  ( 0.000000000000000000, 5.280167904461722905, 3.922743398397384063 ) ) ;
#5105 = ADVANCED_FACE ( 'NONE', ( #12459 ), #7430, .T. ) ;
#5106 = ORIENTED_EDGE ( 'NONE', *, *, #7627, .T. ) ;
#5107 = DIRECTION ( 'NONE',  ( -1.000000000000000000, 1.010728034814421376E-30, 1.090846720500930387E-30 ) ) ;
#5108 = CARTESIAN_POINT ( 'NONE',  ( 11.00000000000001599, 19.99999999999999645, 14.15000000000001812 ) ) ;
#5109 = AXIS2_PLACEMENT_3D ( 'NONE', #10187, #1450, #2495 ) ;
#5110 = DIRECTION ( 'NONE',  ( 0.000000000000000000, 0.000000000000000000, 1.000000000000000000 ) ) ;
#5111 = DIRECTION ( 'NONE',  ( 0.000000000000000000, -0.4999999999999989453, 0.8660254037844391517 ) ) ;
#5112 = CARTESIAN_POINT ( 'NONE',  ( 19.99999999999999645, 2.649444137877595473, 6.020675595748703479 ) ) ;
#5113 = ORIENTED_EDGE ( 'NONE', *, *, #8405, .F. ) ;
#5114 = DIRECTION ( 'NONE',  ( -1.000000000000000000, 1.010728034814421376E-30, 1.090846720500930387E-30 ) ) ;
#5115 = CARTESIAN_POINT ( 'NONE',  ( 0.000000000000000000, -5.492355906873426008, 4.959236492871922586 ) ) ;
#5116 =( NAMED_UNIT ( * ) PLANE_ANGLE_UNIT ( ) SI_UNIT ( $, .RADIAN. ) );
#5117 = VERTEX_POINT ( 'NONE', #12266 ) ;
#5118 = CARTESIAN_POINT ( 'NONE',  ( 40.00000000000000711, 15.24625277455639250, -6.248133273622505257 ) ) ;
#5119 = ORIENTED_EDGE ( 'NONE', *, *, #12552, .F. ) ;
#5120 = ORIENTED_EDGE ( 'NONE', *, *, #12015, .F. ) ;
#5121 = APPLICATION_PROTOCOL_DEFINITION ( 'draft international standard', 'automotive_design', 1998, #10101 ) ;
#5122 = CARTESIAN_POINT ( 'NONE',  ( 14.00000000000000000, 30.00000000000000000, 6.000000000000000000 ) ) ;
#5123 = ORIENTED_EDGE ( 'NONE', *, *, #11983, .F. ) ;
#5124 =( NAMED_UNIT ( * ) SI_UNIT ( $, .STERADIAN. ) SOLID_ANGLE_UNIT ( ) );
#5125 = EDGE_CURVE ( 'NONE', #4694, #962, #8173, .T. ) ;
#5126 = DIRECTION ( 'NONE',  ( -1.000000000000000000, 1.010728034814421376E-30, 1.090846720500930387E-30 ) ) ;
#5127 = VERTEX_POINT ( 'NONE', #8388 ) ;
#5128 = CIRCLE ( 'NONE', #11295, 2.149999999999999023 ) ;
#5129 = AXIS2_PLACEMENT_3D ( 'NONE', #7728, #11596, #1788 ) ;
#5130 =( NAMED_UNIT ( * ) SI_UNIT ( $, .STERADIAN. ) SOLID_ANGLE_UNIT ( ) );
#5131 = DIRECTION ( 'NONE',  ( -1.000000000000000000, -1.031065855027150586E-29, 2.218671295934095703E-30 ) ) ;
#5132 = DIRECTION ( 'NONE',  ( 0.000000000000000000, 0.000000000000000000, -1.000000000000000000 ) ) ;
#5133 = CARTESIAN_POINT ( 'NONE',  ( 2.000000000000001776, 0.000000000000000000, 0.000000000000000000 ) ) ;
#5134 = CIRCLE ( 'NONE', #10036, 2.149999999999992362 ) ;
#5135 = ORIENTED_EDGE ( 'NONE', *, *, #1446, .F. ) ;
#5136 = ORIENTED_EDGE ( 'NONE', *, *, #7236, .T. ) ;
#5137 = ORIENTED_EDGE ( 'NONE', *, *, #9484, .T. ) ;
#5138 = AXIS2_PLACEMENT_3D ( 'NONE', #4116, #1341, #10937 ) ;
#5139 = EDGE_LOOP ( 'NONE', ( #8872, #9117, #2186, #8240 ) ) ;
#5140 = VECTOR ( 'NONE', #1246, 1000.000000000000000 ) ;
#5141 = AXIS2_PLACEMENT_3D ( 'NONE', #1967, #10535, #2710 ) ;
#5142 = DIRECTION ( 'NONE',  ( 1.224646799147352714E-16, 1.177425296209236909E-30, 1.000000000000000000 ) ) ;
#5143 = CARTESIAN_POINT ( 'NONE',  ( 19.99999999999999645, 4.772487208025126826, 4.411390579991361527 ) ) ;
#5144 = VERTEX_POINT ( 'NONE', #11231 ) ;
#5145 = CARTESIAN_POINT ( 'NONE',  ( 4.000000000000000000, 2.309401076758511806, -0.5000000000000038858 ) ) ;
#5146 = ORIENTED_EDGE ( 'NONE', *, *, #11395, .F. ) ;
#5147 = CARTESIAN_POINT ( 'NONE',  ( 19.99999999999999645, 0.000000000000000000, 0.000000000000000000 ) ) ;
#5148 = EDGE_CURVE ( 'NONE', #7570, #11547, #956, .T. ) ;
#5149 = CIRCLE ( 'NONE', #2490, 7.400000000000011902 ) ;
#5150 = EDGE_CURVE ( 'NONE', #701, #1466, #1367, .T. ) ;
#5151 = AXIS2_PLACEMENT_3D ( 'NONE', #6456, #1550, #9580 ) ;
#5152 = VECTOR ( 'NONE', #3309, 1000.000000000000000 ) ;
#5153 = CARTESIAN_POINT ( 'NONE',  ( 0.000000000000000000, -5.932103089875957025, 2.654647609586676005 ) ) ;
#5154 = PRODUCT_DEFINITION_CONTEXT ( 'detailed design', #5918, 'design' ) ;
#5155 = DIRECTION ( 'NONE',  ( 1.000000000000000000, 1.849040895279789448E-31, -6.938893903907224680E-17 ) ) ;
#5156 = VERTEX_POINT ( 'NONE', #9215 ) ;
#5157 = DIRECTION ( 'NONE',  ( -0.000000000000000000, -1.000000000000000000, -0.000000000000000000 ) ) ;
#5158 = ORIENTED_EDGE ( 'NONE', *, *, #10844, .T. ) ;
#5159 = CARTESIAN_POINT ( 'NONE',  ( -30.00000000000000000, 0.000000000000000000, 3.477184903947654954E-15 ) ) ;
#5160 =( GEOMETRIC_REPRESENTATION_CONTEXT ( 3 ) GLOBAL_UNCERTAINTY_ASSIGNED_CONTEXT ( ( #11617 ) ) GLOBAL_UNIT_ASSIGNED_CONTEXT ( ( #12424, #11452, #12364 ) ) REPRESENTATION_CONTEXT ( 'NONE', 'WORKASPACE' ) );
#5161 =( NAMED_UNIT ( * ) SI_UNIT ( $, .STERADIAN. ) SOLID_ANGLE_UNIT ( ) );
#5162 = CARTESIAN_POINT ( 'NONE',  ( -31.74999999999995026, 0.000000000000000000, 6.938893903907228378E-15 ) ) ;
#5163 = FACE_OUTER_BOUND ( 'NONE', #8488, .T. ) ;
#5164 = PRODUCT_DEFINITION ( 'UNKNOWN', '', #2210, #9661 ) ;
#5165 = CARTESIAN_POINT ( 'NONE',  ( 0.000000000000000000, 6.359534927042314045, 1.339147681075194996 ) ) ;
#5166 = CARTESIAN_POINT ( 'NONE',  ( 2.000000000000091926, 0.8865213383406691516, -1.535500000000002085 ) ) ;
#5167 = DIRECTION ( 'NONE',  ( 0.000000000000000000, 0.000000000000000000, -1.000000000000000000 ) ) ;
#5168 = CARTESIAN_POINT ( 'NONE',  ( 20.00000000000000000, 15.24625277455639072, -6.248133273622503481 ) ) ;
#5169 = CARTESIAN_POINT ( 'NONE',  ( -2.499999999999966249, -3.469446951953614189E-15, -4.974600000000009459 ) ) ;
#5170 = SHAPE_REPRESENTATION_RELATIONSHIP ( 'NONE' , 'NONE' ,  #71, #11261 ) ;
#5171 = AXIS2_PLACEMENT_3D ( 'NONE', #12464, #8585, #2684 ) ;
#5172 = ORIENTED_EDGE ( 'NONE', *, *, #6084, .T. ) ;
#5173 = CARTESIAN_POINT ( 'NONE',  ( 0.000000000000000000, -2.401522331692917511, 6.999477872697379865 ) ) ;
#5174 = DIRECTION ( 'NONE',  ( 1.000000000000000000, 0.000000000000000000, 0.000000000000000000 ) ) ;
#5175 = LINE ( 'NONE', #12007, #4886 ) ;
#5176 = ADVANCED_FACE ( 'NONE', ( #403 ), #4334, .T. ) ;
#5177 = DIRECTION ( 'NONE',  ( -1.848892746611746419E-31, -1.000000000000000000, 3.250006781153460502E-32 ) ) ;
#5178 = ORIENTED_EDGE ( 'NONE', *, *, #5856, .F. ) ;
#5179 = CARTESIAN_POINT ( 'NONE',  ( 33.00000000000001421, 40.41548023366553366, -10.14535464186970870 ) ) ;
#5180 = EDGE_CURVE ( 'NONE', #5074, #6567, #3247, .T. ) ;
#5181 = CIRCLE ( 'NONE', #1470, 7.400000000000011902 ) ;
#5182 = CARTESIAN_POINT ( 'NONE',  ( 19.99999999999999645, -4.999339924971525129, -4.274890546384038537 ) ) ;
#5183 = EDGE_CURVE ( 'NONE', #8136, #9222, #1984, .T. ) ;
#5184 = VECTOR ( 'NONE', #5418, 1000.000000000000000 ) ;
#5185 = ORIENTED_EDGE ( 'NONE', *, *, #11482, .T. ) ;
#5186 = EDGE_CURVE ( 'NONE', #3305, #2119, #3648, .T. ) ;
#5187 = DIRECTION ( 'NONE',  ( -1.000000000000000000, 1.010728034814421376E-30, 1.090846720500930387E-30 ) ) ;
#5188 = ORIENTED_EDGE ( 'NONE', *, *, #2751, .T. ) ;
#5189 = ORIENTED_EDGE ( 'NONE', *, *, #10805, .T. ) ;
#5190 = DIRECTION ( 'NONE',  ( 1.000000000000000000, -1.010728034814421376E-30, -1.090846720500930387E-30 ) ) ;
#5191 = ORIENTED_EDGE ( 'NONE', *, *, #1757, .T. ) ;
#5192 =( NAMED_UNIT ( * ) SI_UNIT ( $, .STERADIAN. ) SOLID_ANGLE_UNIT ( ) );
#5193 = CARTESIAN_POINT ( 'NONE',  ( 40.00000000000006395, 1.290960574571364216E-15, -20.00000000000000000 ) ) ;
#5194 = CIRCLE ( 'NONE', #3361, 7.400000000000011902 ) ;
#5195 = ORIENTED_EDGE ( 'NONE', *, *, #10728, .T. ) ;
#5196 = CARTESIAN_POINT ( 'NONE',  ( 15.00000000000003375, 12.50000000000000000, 4.000000000000000000 ) ) ;
#5197 = DIRECTION ( 'NONE',  ( -1.000000000000000000, 1.010728034814421376E-30, 1.090846720500930387E-30 ) ) ;
#5198 = CARTESIAN_POINT ( 'NONE',  ( 19.99999999999999645, 2.520781513113643513, 6.075668640744193105 ) ) ;
#5199 = ORIENTED_EDGE ( 'NONE', *, *, #11225, .T. ) ;
#5200 = ORIENTED_EDGE ( 'NONE', *, *, #9825, .F. ) ;
#5201 = CIRCLE ( 'NONE', #7672, 6.000000000000000000 ) ;
#5202 = ORIENTED_EDGE ( 'NONE', *, *, #1472, .T. ) ;
#5203 = AXIS2_PLACEMENT_3D ( 'NONE', #8158, #5205, #10269 ) ;
#5204 = VERTEX_POINT ( 'NONE', #5743 ) ;
#5205 = DIRECTION ( 'NONE',  ( 1.000000000000000000, -6.162975822039154730E-33, -4.563833282352349791E-17 ) ) ;
#5206 = CARTESIAN_POINT ( 'NONE',  ( 4.000000000000001776, 1.680228229147209040, -3.316631783031879444 ) ) ;
#5207 = ORIENTED_EDGE ( 'NONE', *, *, #11737, .F. ) ;
#5208 = DIRECTION ( 'NONE',  ( 1.000000000000000000, 1.081682119347366197E-16, -6.938893903907228378E-17 ) ) ;
#5209 = EDGE_LOOP ( 'NONE', ( #2250, #11125 ) ) ;
#5210 = CIRCLE ( 'NONE', #9102, 7.400000000000011902 ) ;
#5211 = CYLINDRICAL_SURFACE ( 'NONE', #5433, 2.800000000000003819 ) ;
#5212 = VECTOR ( 'NONE', #305, 1000.000000000000000 ) ;
#5213 = CARTESIAN_POINT ( 'NONE',  ( 0.000000000000000000, -5.362766118793832248, -3.671204237728701969 ) ) ;
#5214 = CARTESIAN_POINT ( 'NONE',  ( 2.000000000000001776, -1.773042676681341856, 3.469446951953614189E-15 ) ) ;
#5215 = ORIENTED_EDGE ( 'NONE', *, *, #9098, .F. ) ;
#5216 = CARTESIAN_POINT ( 'NONE',  ( 19.99999999999999645, -4.357840574720623472, 4.821434073521965402 ) ) ;
#5217 = EDGE_LOOP ( 'NONE', ( #11701, #3199, #3068, #3244, #2421, #7025, #1199, #6196 ) ) ;
#5218 = CARTESIAN_POINT ( 'NONE',  ( 19.99999999999997868, 1.834336845376804748, -6.234758161925229913 ) ) ;
#5219 = EDGE_CURVE ( 'NONE', #1374, #9285, #3847, .T. ) ;
#5220 =( NAMED_UNIT ( * ) SI_UNIT ( $, .STERADIAN. ) SOLID_ANGLE_UNIT ( ) );
#5221 = PLANE ( 'NONE',  #2706 ) ;
#5222 = DIRECTION ( 'NONE',  ( 0.000000000000000000, 0.000000000000000000, -1.000000000000000000 ) ) ;
#5223 = CIRCLE ( 'NONE', #3591, 7.400000000000011902 ) ;
#5224 = DIRECTION ( 'NONE',  ( 1.238279320584846685E-16, -0.9554649393887558739, 0.2951046417778634412 ) ) ;
#5225 = DIRECTION ( 'NONE',  ( -1.154721252774410375E-34, -3.250006781153453386E-32, 1.000000000000000000 ) ) ;
#5226 = LINE ( 'NONE', #5286, #8414 ) ;
#5227 = DIRECTION ( 'NONE',  ( -1.000000000000000000, 1.010728034814421376E-30, 1.090846720500930387E-30 ) ) ;
#5228 = CIRCLE ( 'NONE', #4199, 2.800000000000003819 ) ;
#5229 = CARTESIAN_POINT ( 'NONE',  ( 19.99999999999999645, -5.362766118793865111, 3.671204237728611819 ) ) ;
#5230 = EDGE_CURVE ( 'NONE', #222, #10385, #10468, .T. ) ;
#5231 = EDGE_CURVE ( 'NONE', #4489, #12605, #11669, .T. ) ;
#5232 = EDGE_CURVE ( 'NONE', #11765, #6098, #9585, .T. ) ;
#5233 = ORIENTED_EDGE ( 'NONE', *, *, #6278, .T. ) ;
#5234 = DIRECTION ( 'NONE',  ( -1.238279320584846685E-16, 0.9554649393887558739, -0.2951046417778634412 ) ) ;
#5235 = CYLINDRICAL_SURFACE ( 'NONE', #6242, 14.99999999999998757 ) ;
#5236 = CARTESIAN_POINT ( 'NONE',  ( -4.204114297095544295, 1.660363174096594951, -3.602136431857922982 ) ) ;
#5237 = CARTESIAN_POINT ( 'NONE',  ( 4.000000000000003553, 4.286263797015725748E-16, -3.500000000000000000 ) ) ;
#5238 = CIRCLE ( 'NONE', #1745, 7.400000000000011902 ) ;
#5239 = CARTESIAN_POINT ( 'NONE',  ( 19.99999999999997868, -2.099089055167727480, -6.233932467347804263 ) ) ;
#5240 = LINE ( 'NONE', #10238, #7707 ) ;
#5241 = PRODUCT ( 'socket head cap screw_iso_ISO 4762 M4 x 30 - 20N', 'socket head cap screw_iso_ISO 4762 M4 x 30 - 20N', '', ( #2025 ) ) ;
#5242 = ORIENTED_EDGE ( 'NONE', *, *, #8637, .F. ) ;
#5243 = DIRECTION ( 'NONE',  ( 1.000000000000000000, 1.849040895279789448E-31, -6.938893903907224680E-17 ) ) ;
#5244 = VERTEX_POINT ( 'NONE', #910 ) ;
#5245 = CIRCLE ( 'NONE', #3615, 6.499000000000009436 ) ;
#5246 = ORIENTED_EDGE ( 'NONE', *, *, #10436, .T. ) ;
#5247 = ITEM_DEFINED_TRANSFORMATION ( 'NONE', 'NONE', #10830,  #12422 ) ;
#5248 = ORIENTED_EDGE ( 'NONE', *, *, #2724, .F. ) ;
#5249 = DIRECTION ( 'NONE',  ( -4.930380657631325535E-31, -1.000000000000000000, -1.177425296209239362E-30 ) ) ;
#5250 = CARTESIAN_POINT ( 'NONE',  ( -17.00000000000000000, 2.531464386849858155E-30, 22.15000000000007319 ) ) ;
#5251 = CARTESIAN_POINT ( 'NONE',  ( 4.211140560182196069, 2.431303136016537358, -3.745885042887416638 ) ) ;
#5252 = CARTESIAN_POINT ( 'NONE',  ( 0.000000000000000000, 0.000000000000000000, 0.000000000000000000 ) ) ;
#5253 = ADVANCED_FACE ( 'NONE', ( #8647 ), #4906, .T. ) ;
#5254 = CARTESIAN_POINT ( 'NONE',  ( 4.197393957002303999, 7.389034437926038210E-14, -3.503767560748934251 ) ) ;
#5255 = DIRECTION ( 'NONE',  ( -0.000000000000000000, -1.000000000000000000, -0.000000000000000000 ) ) ;
#5256 = ORIENTED_EDGE ( 'NONE', *, *, #10360, .T. ) ;
#5257 = VERTEX_POINT ( 'NONE', #1879 ) ;
#5258 = ORIENTED_EDGE ( 'NONE', *, *, #368, .T. ) ;
#5259 = ORIENTED_EDGE ( 'NONE', *, *, #9720, .F. ) ;
#5260 = ADVANCED_FACE ( 'NONE', ( #12648 ), #8580, .T. ) ;
#5261 = DIRECTION ( 'NONE',  ( 1.238279320584846685E-16, -0.9554649393887560960, 0.2951046417778627751 ) ) ;
#5262 = EDGE_CURVE ( 'NONE', #12512, #10385, #6161, .T. ) ;
#5263 = CARTESIAN_POINT ( 'NONE',  ( 0.1756481739660588626, -4.720212674039006906, -3.469390959564082166 ) ) ;
#5264 = ORIENTED_EDGE ( 'NONE', *, *, #6419, .F. ) ;
#5265 = APPLICATION_CONTEXT ( 'automotive_design' ) ;
#5266 = CIRCLE ( 'NONE', #10178, 10.00000000000000178 ) ;
#5267 = CARTESIAN_POINT ( 'NONE',  ( 0.000000000000000000, 30.00000000000000000, -7.999999999999998224 ) ) ;
#5268 = ORIENTED_EDGE ( 'NONE', *, *, #2120, .T. ) ;
#5269 = CARTESIAN_POINT ( 'NONE',  ( 9.000000000000035527, -19.99999999999999645, 12.00000000000003553 ) ) ;
#5270 = CARTESIAN_POINT ( 'NONE',  ( -18.00000000000002842, 30.00000000000000000, 2.000000000000004441 ) ) ;
#5271 = DIRECTION ( 'NONE',  ( -1.000000000000000000, -1.081682119347366197E-16, 6.938893903907228378E-17 ) ) ;
#5272 = VECTOR ( 'NONE', #11503, 1000.000000000000000 ) ;
#5273 = CARTESIAN_POINT ( 'NONE',  ( 27.00000000000000355, 39.34792583643766051, -19.21347054209566707 ) ) ;
#5274 = AXIS2_PLACEMENT_3D ( 'NONE', #10520, #2618, #5509 ) ;
#5275 = ORIENTED_EDGE ( 'NONE', *, *, #12168, .F. ) ;
#5276 = ORIENTED_EDGE ( 'NONE', *, *, #3773, .T. ) ;
#5277 = DIRECTION ( 'NONE',  ( 1.000000000000000000, -0.000000000000000000, -0.000000000000000000 ) ) ;
#5278 = ADVANCED_FACE ( 'NONE', ( #5803 ), #15, .F. ) ;
#5279 = CARTESIAN_POINT ( 'NONE',  ( 0.000000000000000000, 0.8865213383406727043, 1.535499999999998755 ) ) ;
#5280 = VECTOR ( 'NONE', #7864, 1000.000000000000000 ) ;
#5281 = DIRECTION ( 'NONE',  ( 1.000000000000000000, 5.916456789157575403E-31, -1.577021341797098793E-16 ) ) ;
#5282 = CIRCLE ( 'NONE', #1369, 2.800000000000003819 ) ;
#5283 = EDGE_CURVE ( 'NONE', #8740, #711, #6849, .T. ) ;
#5284 = CARTESIAN_POINT ( 'NONE',  ( 0.000000000000000000, 3.975087478966741639, -6.241688836730176604 ) ) ;
#5285 = DIRECTION ( 'NONE',  ( -1.000000000000000000, 1.010728034814421376E-30, 1.090846720500930387E-30 ) ) ;
#5286 = CARTESIAN_POINT ( 'NONE',  ( 9.999999999999998224, 7.358375340957004518, -0.7837807994560894720 ) ) ;
#5287 = ORIENTED_EDGE ( 'NONE', *, *, #603, .F. ) ;
#5288 = PRODUCT_DEFINITION_FORMATION_WITH_SPECIFIED_SOURCE ( 'ANY', '', #2588, .NOT_KNOWN. ) ;
#5289 = CARTESIAN_POINT ( 'NONE',  ( 0.000000000000000000, 6.557268578288196537, 0.5199208220222142351 ) ) ;
#5290 = AXIS2_PLACEMENT_3D ( 'NONE', #5928, #9970, #9141 ) ;
#5291 = AXIS2_PLACEMENT_3D ( 'NONE', #7957, #3340, #10189 ) ;
#5292 = CARTESIAN_POINT ( 'NONE',  ( 0.000000000000000000, 6.718789039999951029, 3.101269713516811688 ) ) ;
#5293 = EDGE_CURVE ( 'NONE', #1397, #8559, #12711, .T. ) ;
#5294 = ORIENTED_EDGE ( 'NONE', *, *, #1838, .F. ) ;
#5295 = CARTESIAN_POINT ( 'NONE',  ( 19.99999999999999645, -3.399584271718382844, 6.572885726945580487 ) ) ;
#5296 = CARTESIAN_POINT ( 'NONE',  ( -7.321615276582520023E-30, 2.276419975238227341E-16, -3.299999999999999822 ) ) ;
#5297 = CARTESIAN_POINT ( 'NONE',  ( -17.00000000000002842, -20.00000000000000000, 12.00000000000003730 ) ) ;
#5298 = LINE ( 'NONE', #4532, #2846 ) ;
#5299 = EDGE_CURVE ( 'NONE', #9551, #12099, #10625, .T. ) ;
#5300 = CARTESIAN_POINT ( 'NONE',  ( 40.00000000000000000, 39.34792583643765340, -17.06347054209567560 ) ) ;
#5301 = EDGE_CURVE ( 'NONE', #3242, #9611, #140, .T. ) ;
#5302 = DIRECTION ( 'NONE',  ( 1.000000000000000000, 1.081682119347366197E-16, -6.938893903907228378E-17 ) ) ;
#5303 = SURFACE_STYLE_FILL_AREA ( #1371 ) ;
#5304 = VERTEX_POINT ( 'NONE', #7922 ) ;
#5305 = FACE_OUTER_BOUND ( 'NONE', #12480, .T. ) ;
#5306 = ORIENTED_EDGE ( 'NONE', *, *, #4448, .F. ) ;
#5307 = EDGE_LOOP ( 'NONE', ( #7877, #10476, #9366, #2913 ) ) ;
#5308 = CIRCLE ( 'NONE', #4729, 19.99999999999998934 ) ;
#5309 = VERTEX_POINT ( 'NONE', #11932 ) ;
#5310 = CARTESIAN_POINT ( 'NONE',  ( -1.144235203016672475, -3.958177651039087586, -0.09382832055445461394 ) ) ;
#5311 = CYLINDRICAL_SURFACE ( 'NONE', #4804, 2.149999999999999023 ) ;
#5312 =( LENGTH_UNIT ( ) NAMED_UNIT ( * ) SI_UNIT ( .MILLI., .METRE. ) );
#5313 = FACE_OUTER_BOUND ( 'NONE', #4323, .T. ) ;
#5314 = CARTESIAN_POINT ( 'NONE',  ( 19.99999999999997868, 6.424561140605085541, 0.9808237102697028309 ) ) ;
#5315 = ORIENTED_EDGE ( 'NONE', *, *, #8229, .T. ) ;
#5316 = DIRECTION ( 'NONE',  ( -1.000000000000000000, 1.010728034814421376E-30, 1.090846720500930387E-30 ) ) ;
#5317 = EDGE_CURVE ( 'NONE', #9583, #2582, #6733, .T. ) ;
#5318 = CARTESIAN_POINT ( 'NONE',  ( -15.00000000000000000, 30.00000000000000000, 3.000000000000029754 ) ) ;
#5319 = ORIENTED_EDGE ( 'NONE', *, *, #10552, .F. ) ;
#5320 = ORIENTED_EDGE ( 'NONE', *, *, #9493, .T. ) ;
#5321 = ORIENTED_EDGE ( 'NONE', *, *, #450, .T. ) ;
#5322 = VERTEX_POINT ( 'NONE', #6058 ) ;
#5323 = DIRECTION ( 'NONE',  ( -1.387778780781445182E-16, 0.9997704357740726522, 0.02142605311579142552 ) ) ;
#5324 = EDGE_CURVE ( 'NONE', #10180, #8458, #11806, .T. ) ;
#5325 = EDGE_CURVE ( 'NONE', #1822, #5778, #10819, .T. ) ;
#5326 = AXIS2_PLACEMENT_3D ( 'NONE', #1776, #2769, #6808 ) ;
#5327 = AXIS2_PLACEMENT_3D ( 'NONE', #4825, #10670, #5722 ) ;
#5328 = EDGE_LOOP ( 'NONE', ( #6049, #9961, #7266, #5505 ) ) ;
#5329 = DIRECTION ( 'NONE',  ( 0.000000000000000000, 1.000000000000000000, 0.000000000000000000 ) ) ;
#5330 = ORIENTED_EDGE ( 'NONE', *, *, #2666, .F. ) ;
#5331 = CARTESIAN_POINT ( 'NONE',  ( -3.680118525130247509, 2.494084732383328173, -0.3507732604232469131 ) ) ;
#5332 = LINE ( 'NONE', #3297, #10153 ) ;
#5333 = EDGE_CURVE ( 'NONE', #2941, #3905, #12075, .T. ) ;
#5334 = DIRECTION ( 'NONE',  ( 1.140150527077241698E-30, 0.000000000000000000, -1.000000000000000000 ) ) ;
#5335 = EDGE_CURVE ( 'NONE', #11717, #11591, #11018, .T. ) ;
#5336 = AXIS2_PLACEMENT_3D ( 'NONE', #9785, #11934, #914 ) ;
#5337 =( GEOMETRIC_REPRESENTATION_CONTEXT ( 3 ) GLOBAL_UNCERTAINTY_ASSIGNED_CONTEXT ( ( #9534 ) ) GLOBAL_UNIT_ASSIGNED_CONTEXT ( ( #1882, #6665, #10572 ) ) REPRESENTATION_CONTEXT ( 'NONE', 'WORKASPACE' ) );
#5338 = AXIS2_PLACEMENT_3D ( 'NONE', #10368, #1555, #8445 ) ;
#5339 = CYLINDRICAL_SURFACE ( 'NONE', #2897, 2.149999999999999023 ) ;
#5340 = ORIENTED_EDGE ( 'NONE', *, *, #12250, .F. ) ;
#5341 = CIRCLE ( 'NONE', #11314, 2.800000000000003375 ) ;
#5342 = ORIENTED_EDGE ( 'NONE', *, *, #9702, .F. ) ;
#5343 = DIRECTION ( 'NONE',  ( -0.000000000000000000, -1.000000000000000000, -0.000000000000000000 ) ) ;
#5344 = EDGE_CURVE ( 'NONE', #1618, #6292, #1587, .T. ) ;
#5345 = DIRECTION ( 'NONE',  ( 0.000000000000000000, 0.000000000000000000, 1.000000000000000000 ) ) ;
#5346 = VECTOR ( 'NONE', #771, 1000.000000000000000 ) ;
#5347 = CIRCLE ( 'NONE', #820, 6.499000000000006771 ) ;
#5348 = DIRECTION ( 'NONE',  ( 0.000000000000000000, 0.000000000000000000, 1.000000000000000000 ) ) ;
#5349 = LINE ( 'NONE', #5478, #3835 ) ;
#5350 = FACE_OUTER_BOUND ( 'NONE', #5999, .T. ) ;
#5351 = DIRECTION ( 'NONE',  ( 0.000000000000000000, 0.000000000000000000, 1.000000000000000000 ) ) ;
#5352 = ORIENTED_EDGE ( 'NONE', *, *, #2077, .T. ) ;
#5354 = CARTESIAN_POINT ( 'NONE',  ( 3.333333333333334814, 2.694301256218240237, -3.300726591567062940 ) ) ;
#5353 = COLOUR_RGB ( '', 0.31764706, 0.68627451, 0.89019608) ;
#5355 = AXIS2_PLACEMENT_3D ( 'NONE', #932, #4742, #12669 ) ;
#5356 = VECTOR ( 'NONE', #3984, 1000.000000000000000 ) ;
#5357 = DIRECTION ( 'NONE',  ( 0.000000000000000000, 0.000000000000000000, -1.000000000000000000 ) ) ;
#5358 = ORIENTED_EDGE ( 'NONE', *, *, #7431, .F. ) ;
#5359 = CARTESIAN_POINT ( 'NONE',  ( -17.00000000000002842, 19.99999999999998579, 12.00000000000003730 ) ) ;
#5360 = CYLINDRICAL_SURFACE ( 'NONE', #3382, 2.800000000000003819 ) ;
#5361 =( GEOMETRIC_REPRESENTATION_CONTEXT ( 3 ) GLOBAL_UNCERTAINTY_ASSIGNED_CONTEXT ( ( #4692 ) ) GLOBAL_UNIT_ASSIGNED_CONTEXT ( ( #10289, #8306, #4445 ) ) REPRESENTATION_CONTEXT ( 'NONE', 'WORKASPACE' ) );
#5362 = CARTESIAN_POINT ( 'NONE',  ( 3.469446951953614189E-15, 4.618802153517009401, -0.5000000000000091038 ) ) ;
#5363 = CARTESIAN_POINT ( 'NONE',  ( 4.101954839143211906, -2.368264730583032218, -3.681130640444385982 ) ) ;
#5364 = DIRECTION ( 'NONE',  ( 0.000000000000000000, -0.7818314824680222541, -0.6234898018587429203 ) ) ;
#5365 = DIRECTION ( 'NONE',  ( 0.000000000000000000, 0.000000000000000000, -1.000000000000000000 ) ) ;
#5366 = PLANE ( 'NONE',  #12549 ) ;
#5367 = EDGE_LOOP ( 'NONE', ( #11973, #4960, #3085, #989 ) ) ;
#5368 = CARTESIAN_POINT ( 'NONE',  ( 20.00000000000000000, 9.907988025913237351, -23.58742161290648554 ) ) ;
#5369 = VERTEX_POINT ( 'NONE', #5165 ) ;
#5370 = AXIS2_PLACEMENT_3D ( 'NONE', #1309, #5434, #9286 ) ;
#5371 = ORIENTED_EDGE ( 'NONE', *, *, #4230, .T. ) ;
#5372 = EDGE_CURVE ( 'NONE', #11663, #11879, #12086, .T. ) ;
#5373 = ORIENTED_EDGE ( 'NONE', *, *, #4614, .T. ) ;
#5374 = FILL_AREA_STYLE_COLOUR ( '', #5938 ) ;
#5375 = DIRECTION ( 'NONE',  ( -1.140150527077241873E-30, 0.000000000000000000, 1.000000000000000000 ) ) ;
#5376 = CYLINDRICAL_SURFACE ( 'NONE', #1567, 4.000000000000008882 ) ;
#5377 = CYLINDRICAL_SURFACE ( 'NONE', #1426, 9.999999999999998224 ) ;
#5378 = AXIS2_PLACEMENT_3D ( 'NONE', #8707, #778, #2802 ) ;
#5379 = CARTESIAN_POINT ( 'NONE',  ( 0.000000000000000000, -1.773042676681359175, 1.387778780781445676E-14 ) ) ;
#5380 = ORIENTED_EDGE ( 'NONE', *, *, #1749, .T. ) ;
#5381 = CARTESIAN_POINT ( 'NONE',  ( 0.1999999999999987899, 2.209466446554762247E-16, -3.300000000000003375 ) ) ;
#5382 = CIRCLE ( 'NONE', #12189, 4.000000000000000000 ) ;
#5383 = CARTESIAN_POINT ( 'NONE',  ( 0.1999999999999987899, 1.942890293094023946E-16, 3.500000000000003997 ) ) ;
#5384 = ORIENTED_EDGE ( 'NONE', *, *, #8895, .F. ) ;
#5385 = ORIENTED_EDGE ( 'NONE', *, *, #3310, .F. ) ;
#5386 = ORIENTED_EDGE ( 'NONE', *, *, #3942, .F. ) ;
#5387 = ORIENTED_EDGE ( 'NONE', *, *, #5468, .T. ) ;
#5388 = FACE_OUTER_BOUND ( 'NONE', #6348, .T. ) ;
#5389 = VECTOR ( 'NONE', #9457, 1000.000000000000000 ) ;
#5390 = ADVANCED_FACE ( 'NONE', ( #2136 ), #327, .T. ) ;
#5391 = DIRECTION ( 'NONE',  ( -1.848892746611746419E-31, -1.000000000000000000, 3.250006781153460502E-32 ) ) ;
#5392 = PRODUCT_DEFINITION ( 'UNKNOWN', '', #3856, #11070 ) ;
#5393 = ORIENTED_EDGE ( 'NONE', *, *, #6245, .F. ) ;
#5394 = FACE_OUTER_BOUND ( 'NONE', #8377, .T. ) ;
#5395 = EDGE_LOOP ( 'NONE', ( #11182, #8165, #6920 ) ) ;
#5396 = CARTESIAN_POINT ( 'NONE',  ( 19.99999999999997868, 5.956456411769428527, -2.790827096698922372 ) ) ;
#5397 = DIRECTION ( 'NONE',  ( -2.465190328815656418E-32, 1.177425296209236734E-30, 1.000000000000000000 ) ) ;
#5398 = EDGE_CURVE ( 'NONE', #4508, #10621, #1098, .T. ) ;
#5399 = CARTESIAN_POINT ( 'NONE',  ( -16.99999999999999289, -30.00000000000000000, 25.00000000000007105 ) ) ;
#5400 = AXIS2_PLACEMENT_3D ( 'NONE', #12566, #2853, #1602 ) ;
#5401 = DIRECTION ( 'NONE',  ( -1.000000000000000000, 1.010728034814421376E-30, 1.090846720500930387E-30 ) ) ;
#5402 = ORIENTED_EDGE ( 'NONE', *, *, #7036, .F. ) ;
#5403 = VERTEX_POINT ( 'NONE', #9843 ) ;
#5404 = CARTESIAN_POINT ( 'NONE',  ( -35.00000000000006395, 30.00000000000000000, 2.218822049206179977E-15 ) ) ;
#5405 = EDGE_CURVE ( 'NONE', #6222, #803, #7033, .T. ) ;
#5406 = VECTOR ( 'NONE', #11160, 1000.000000000000000 ) ;
#5407 = LINE ( 'NONE', #9512, #2887 ) ;
#5408 = AXIS2_PLACEMENT_3D ( 'NONE', #8288, #3350, #7332 ) ;
#5409 = EDGE_CURVE ( 'NONE', #2245, #9520, #8168, .T. ) ;
#5410 = DIRECTION ( 'NONE',  ( -1.000000000000000000, 1.010728034814421376E-30, 1.090846720500930387E-30 ) ) ;
#5411 = DIRECTION ( 'NONE',  ( 1.000000000000000000, -1.010728034814421376E-30, -1.090846720500930387E-30 ) ) ;
#5412 = ADVANCED_FACE ( 'NONE', ( #5099 ), #4884, .F. ) ;
#5413 = CARTESIAN_POINT ( 'NONE',  ( 0.000000000000000000, 0.000000000000000000, 0.000000000000000000 ) ) ;
#5414 = AXIS2_PLACEMENT_3D ( 'NONE', #2493, #5442, #7320 ) ;
#5415 = PLANE ( 'NONE',  #10469 ) ;
#5416 = VERTEX_POINT ( 'NONE', #9906 ) ;
#5417 = CARTESIAN_POINT ( 'NONE',  ( 2.000000000000013323, 3.464101615137772150, -3.142992957459230574 ) ) ;
#5418 = DIRECTION ( 'NONE',  ( 1.000000000000000000, -1.010728034814421376E-30, -1.090846720500930387E-30 ) ) ;
#5419 = EDGE_CURVE ( 'NONE', #10664, #11692, #12011, .T. ) ;
#5420 = ADVANCED_FACE ( 'NONE', ( #11993 ), #8887, .T. ) ;
#5421 = CARTESIAN_POINT ( 'NONE',  ( 33.00000000000001421, 39.34792583643766761, -14.56347054209569158 ) ) ;
#5422 = AXIS2_PLACEMENT_3D ( 'NONE', #6530, #401, #4398 ) ;
#5423 = ORIENTED_EDGE ( 'NONE', *, *, #5431, .T. ) ;
#5424 = DIRECTION ( 'NONE',  ( -1.000000000000000000, 1.010728034814421376E-30, 1.090846720500930387E-30 ) ) ;
#5425 = CARTESIAN_POINT ( 'NONE',  ( 19.99999999999999645, -5.148708580507705967, 3.965829163366258570 ) ) ;
#5426 = FACE_OUTER_BOUND ( 'NONE', #10558, .T. ) ;
#5427 = CARTESIAN_POINT ( 'NONE',  ( 2.804994570502159057, 3.229033611042447571, -3.526374918436837813 ) ) ;
#5428 = CARTESIAN_POINT ( 'NONE',  ( 33.61000000000001364, 0.000000000000000000, 0.000000000000000000 ) ) ;
#5429 = CIRCLE ( 'NONE', #11614, 3.999999999999997335 ) ;
#5430 = DIRECTION ( 'NONE',  ( -1.031065855027149465E-29, -1.000000000000000000, 7.771561172376086908E-16 ) ) ;
#5431 = EDGE_CURVE ( 'NONE', #815, #4292, #352, .T. ) ;
#5432 =( LENGTH_UNIT ( ) NAMED_UNIT ( * ) SI_UNIT ( .MILLI., .METRE. ) );
#5433 = AXIS2_PLACEMENT_3D ( 'NONE', #12110, #9127, #9189 ) ;
#5434 = DIRECTION ( 'NONE',  ( -1.159061634649218351E-16, 0.000000000000000000, -1.000000000000000000 ) ) ;
#5435 = ORIENTED_EDGE ( 'NONE', *, *, #9372, .F. ) ;
#5436 = ITEM_DEFINED_TRANSFORMATION ( 'NONE', 'NONE', #4259,  #12422 ) ;
#5437 = CIRCLE ( 'NONE', #12650, 7.999999999999998224 ) ;
#5438 = EDGE_LOOP ( 'NONE', ( #3032, #7643, #7528, #8879 ) ) ;
#5439 = CIRCLE ( 'NONE', #4828, 6.000000000000000000 ) ;
#5440 = VERTEX_POINT ( 'NONE', #1223 ) ;
#5441 = EDGE_CURVE ( 'NONE', #2015, #12512, #3868, .T. ) ;
#5442 = DIRECTION ( 'NONE',  ( 1.159061634649218351E-16, -0.000000000000000000, 1.000000000000000000 ) ) ;
#5443 = CARTESIAN_POINT ( 'NONE',  ( 14.00000000000000000, -12.99999999999999822, 0.000000000000000000 ) ) ;
#5444 = DIRECTION ( 'NONE',  ( 0.000000000000000000, 0.000000000000000000, -1.000000000000000000 ) ) ;
#5445 = LINE ( 'NONE', #9354, #10814 ) ;
#5446 = ORIENTED_EDGE ( 'NONE', *, *, #1224, .F. ) ;
#5447 = EDGE_CURVE ( 'NONE', #10646, #3356, #12707, .T. ) ;
#5448 = CARTESIAN_POINT ( 'NONE',  ( 19.99999999999999645, 0.000000000000000000, 0.000000000000000000 ) ) ;
#5449 = DIRECTION ( 'NONE',  ( 0.000000000000000000, 0.000000000000000000, 1.000000000000000000 ) ) ;
#5450 = ORIENTED_EDGE ( 'NONE', *, *, #8947, .F. ) ;
#5451 = AXIS2_PLACEMENT_3D ( 'NONE', #3869, #5728, #4961 ) ;
#5452 = AXIS2_PLACEMENT_3D ( 'NONE', #11950, #11756, #4859 ) ;
#5453 = ORIENTED_EDGE ( 'NONE', *, *, #11184, .T. ) ;
#5454 = DIRECTION ( 'NONE',  ( -6.938893903907224680E-17, 3.250006781153453386E-32, -1.000000000000000000 ) ) ;
#5455 = VERTEX_POINT ( 'NONE', #2396 ) ;
#5456 = ORIENTED_EDGE ( 'NONE', *, *, #12718, .T. ) ;
#5457 = DIRECTION ( 'NONE',  ( 0.000000000000000000, 0.000000000000000000, -1.000000000000000000 ) ) ;
#5458 = ORIENTED_EDGE ( 'NONE', *, *, #9702, .T. ) ;
#5459 = CARTESIAN_POINT ( 'NONE',  ( 1.999999999999994893, -1.329782007511007169, -0.7677499999999976010 ) ) ;
#5460 = CARTESIAN_POINT ( 'NONE',  ( 9.999999999999994671, 0.2110513566293444054, 7.396989747516548697 ) ) ;
#5461 = ORIENTED_EDGE ( 'NONE', *, *, #7308, .F. ) ;
#5462 = CIRCLE ( 'NONE', #12671, 6.499000000000008548 ) ;
#5463 = AXIS2_PLACEMENT_3D ( 'NONE', #5239, #7114, #4144 ) ;
#5464 = FACE_OUTER_BOUND ( 'NONE', #11198, .T. ) ;
#5465 = CARTESIAN_POINT ( 'NONE',  ( 0.000000000000000000, 3.908107171477168684, 5.192658214849952714 ) ) ;
#5466 = EDGE_CURVE ( 'NONE', #3837, #7377, #10833, .T. ) ;
#5467 = DIRECTION ( 'NONE',  ( 1.000000000000000000, -1.010728034814421376E-30, -1.090846720500930387E-30 ) ) ;
#5468 = EDGE_CURVE ( 'NONE', #11828, #7505, #3492, .T. ) ;
#5469 = UNCERTAINTY_MEASURE_WITH_UNIT (LENGTH_MEASURE( 1.000000000000000082E-05 ), #2406, 'distance_accuracy_value', 'NONE');
#5470 = EDGE_CURVE ( 'NONE', #1917, #11114, #9192, .T. ) ;
#5471 = DIRECTION ( 'NONE',  ( 1.000000000000000000, 8.881784197001252323E-16, 0.000000000000000000 ) ) ;
#5472 = ORIENTED_EDGE ( 'NONE', *, *, #663, .T. ) ;
#5473 = ORIENTED_EDGE ( 'NONE', *, *, #6786, .F. ) ;
#5474 = AXIS2_PLACEMENT_3D ( 'NONE', #216, #2289, #6202 ) ;
#5475 = DIRECTION ( 'NONE',  ( -1.000000000000000000, 1.010728034814421376E-30, 1.090846720500930387E-30 ) ) ;
#5476 = DIRECTION ( 'NONE',  ( 0.000000000000000000, 0.4338837391175525693, 0.9009688679024219216 ) ) ;
#5477 = CARTESIAN_POINT ( 'NONE',  ( 3.469446951953614189E-15, 4.618802153517009401, -0.5000000000000091038 ) ) ;
#5479 = CIRCLE ( 'NONE', #2407, 7.400000000000011902 ) ;
#5478 = CARTESIAN_POINT ( 'NONE',  ( 50.00005079999998969, 5.204170427930421283E-15, 2.499999999999996447 ) ) ;
#5480 = AXIS2_PLACEMENT_3D ( 'NONE', #10079, #369, #2249 ) ;
#5481 = DIRECTION ( 'NONE',  ( -1.000000000000000000, 1.010728034814421376E-30, 1.090846720500930387E-30 ) ) ;
#5482 = ADVANCED_FACE ( 'NONE', ( #9326 ), #2462, .T. ) ;
#5483 = DIRECTION ( 'NONE',  ( 0.000000000000000000, -0.5000000000000012212, -0.8660254037844380415 ) ) ;
#5484 = ORIENTED_EDGE ( 'NONE', *, *, #5909, .F. ) ;
#5485 = DIRECTION ( 'NONE',  ( 0.000000000000000000, 0.000000000000000000, 1.000000000000000000 ) ) ;
#5486 = LINE ( 'NONE', #5229, #10098 ) ;
#5487 = PRESENTATION_STYLE_ASSIGNMENT (( #10435 ) ) ;
#5488 = AXIS2_PLACEMENT_3D ( 'NONE', #5870, #2744, #9591 ) ;
#5489 = EDGE_CURVE ( 'NONE', #11709, #5204, #6314, .T. ) ;
#5490 = VECTOR ( 'NONE', #11117, 1000.000000000000000 ) ;
#5491 = CARTESIAN_POINT ( 'NONE',  ( 19.99999999999997868, 3.681899619563859360, -5.450844343808918246 ) ) ;
#5492 = VERTEX_POINT ( 'NONE', #2530 ) ;
#5493 = DIRECTION ( 'NONE',  ( 6.938893903907224680E-17, -3.250006781153453386E-32, 1.000000000000000000 ) ) ;
#5494 = CARTESIAN_POINT ( 'NONE',  ( 19.99999999999997868, 5.670261409740700920, -3.175710400084609475 ) ) ;
#5495 = DIRECTION ( 'NONE',  ( 0.000000000000000000, -0.5877852522924802425, 0.8090169943749421222 ) ) ;
#5496 = DIRECTION ( 'NONE',  ( 0.000000000000000000, -1.000000000000000000, 0.000000000000000000 ) ) ;
#5497 = PLANE ( 'NONE',  #9761 ) ;
#5498 = AXIS2_PLACEMENT_3D ( 'NONE', #11345, #9203, #12190 ) ;
#5499 = EDGE_CURVE ( 'NONE', #10207, #11698, #542, .T. ) ;
#5500 = CARTESIAN_POINT ( 'NONE',  ( 4.000000000000000000, 2.309401076758511806, -0.5000000000000038858 ) ) ;
#5501 = VECTOR ( 'NONE', #4596, 1000.000000000000000 ) ;
#5502 = EDGE_CURVE ( 'NONE', #2096, #7387, #5349, .T. ) ;
#5503 = FACE_OUTER_BOUND ( 'NONE', #2492, .T. ) ;
#5504 = VERTEX_POINT ( 'NONE', #10292 ) ;
#5505 = ORIENTED_EDGE ( 'NONE', *, *, #7363, .F. ) ;
#5506 = ORIENTED_EDGE ( 'NONE', *, *, #2499, .T. ) ;
#5507 = VECTOR ( 'NONE', #12620, 1000.000000000000114 ) ;
#5508 = DIRECTION ( 'NONE',  ( 1.140150527077241873E-30, 0.000000000000000000, -1.000000000000000000 ) ) ;
#5509 = DIRECTION ( 'NONE',  ( 0.000000000000000000, 0.000000000000000000, 1.000000000000000000 ) ) ;
#5510 = DIRECTION ( 'NONE',  ( -1.000000000000000000, 0.000000000000000000, 0.000000000000000000 ) ) ;
#5511 = LINE ( 'NONE', #612, #5272 ) ;
#5512 = ORIENTED_EDGE ( 'NONE', *, *, #3146, .F. ) ;
#5513 = CARTESIAN_POINT ( 'NONE',  ( -31.74999999999995026, 0.000000000000000000, 6.938893903907228378E-15 ) ) ;
#5514 = DIRECTION ( 'NONE',  ( -0.7071067811865504593, 0.000000000000000000, -0.7071067811865445751 ) ) ;
#5515 = VERTEX_POINT ( 'NONE', #5284 ) ;
#5516 = EDGE_LOOP ( 'NONE', ( #4869, #8479, #5264, #1537 ) ) ;
#5517 = CARTESIAN_POINT ( 'NONE',  ( 11.00000000000003020, -30.00000000000000000, 9.757543507305644146E-31 ) ) ;
#5518 = ORIENTED_EDGE ( 'NONE', *, *, #4393, .T. ) ;
#5519 = VERTEX_POINT ( 'NONE', #9266 ) ;
#5520 = SHAPE_REPRESENTATION_RELATIONSHIP ( 'NONE' , 'NONE' ,  #8305, #11121 ) ;
#5521 = EDGE_CURVE ( 'NONE', #6863, #144, #6451, .T. ) ;
#5522 =( NAMED_UNIT ( * ) SI_UNIT ( $, .STERADIAN. ) SOLID_ANGLE_UNIT ( ) );
#5523 = VERTEX_POINT ( 'NONE', #8310 ) ;
#5524 = CARTESIAN_POINT ( 'NONE',  ( 4.200000000000001954, 0.000000000000000000, 0.000000000000000000 ) ) ;
#5525 = CARTESIAN_POINT ( 'NONE',  ( 9.285714285714284699, -13.00000000000000000, -3.711537444790451001 ) ) ;
#5526 = EDGE_LOOP ( 'NONE', ( #11382, #5843, #1886, #12256 ) ) ;
#5527 = DIRECTION ( 'NONE',  ( -1.000000000000000000, 1.010728034814421376E-30, 1.090846720500930387E-30 ) ) ;
#5528 = LINE ( 'NONE', #12430, #9538 ) ;
#5529 = AXIS2_PLACEMENT_3D ( 'NONE', #9981, #2775, #1591 ) ;
#5530 = LINE ( 'NONE', #10411, #6701 ) ;
#5531 = CARTESIAN_POINT ( 'NONE',  ( -32.85000000000006537, -2.029837716746816226E-29, 2.000000000000003553 ) ) ;
#5532 = ORIENTED_EDGE ( 'NONE', *, *, #10731, .F. ) ;
#5533 = AXIS2_PLACEMENT_3D ( 'NONE', #4867, #3838, #936 ) ;
#5534 = ORIENTED_EDGE ( 'NONE', *, *, #3040, .F. ) ;
#5535 = DIRECTION ( 'NONE',  ( -1.000000000000000000, -5.916456789157575403E-31, -2.465190328815656418E-32 ) ) ;
#5536 = DIRECTION ( 'NONE',  ( 0.000000000000000000, 0.000000000000000000, 1.000000000000000000 ) ) ;
#5537 = ORIENTED_EDGE ( 'NONE', *, *, #7837, .F. ) ;
#5538 = EDGE_CURVE ( 'NONE', #2941, #11755, #3435, .T. ) ;
#5539 = DIRECTION ( 'NONE',  ( -1.000000000000000000, 1.010728034814421376E-30, 1.090846720500930387E-30 ) ) ;
#5540 = ADVANCED_FACE ( 'NONE', ( #6381 ), #5667, .F. ) ;
#5541 = CARTESIAN_POINT ( 'NONE',  ( -1.655952806101424146, 3.662737355149034979, -1.234974037096769500E-15 ) ) ;
#5542 = AXIS2_PLACEMENT_3D ( 'NONE', #10275, #9248, #4498 ) ;
#5543 = PRESENTATION_LAYER_ASSIGNMENT (  '', '', ( #4724 ) ) ;
#5544 = DIRECTION ( 'NONE',  ( -1.000000000000000000, 1.010728034814421376E-30, 1.090846720500930387E-30 ) ) ;
#5545 = VECTOR ( 'NONE', #11640, 1000.000000000000000 ) ;
#5546 = CARTESIAN_POINT ( 'NONE',  ( 33.00000000000001421, 39.34792583643766761, -24.06347054209567915 ) ) ;
#5547 = ORIENTED_EDGE ( 'NONE', *, *, #9886, .T. ) ;
#5548 = DIRECTION ( 'NONE',  ( -1.140150527077241873E-30, 0.000000000000000000, 1.000000000000000000 ) ) ;
#5549 = CARTESIAN_POINT ( 'NONE',  ( -3.999999999999963585, -2.309401076758515359, -3.433295621305398893 ) ) ;
#5550 = VECTOR ( 'NONE', #9896, 1000.000000000000000 ) ;
#5551 = VECTOR ( 'NONE', #3683, 1000.000000000000000 ) ;
#5552 = AXIS2_PLACEMENT_3D ( 'NONE', #4652, #11420, #2599 ) ;
#5553 = CARTESIAN_POINT ( 'NONE',  ( 19.99999999999999645, 1.395418990828201533, 6.428133065596412621 ) ) ;
#5554 = ADVANCED_FACE ( 'NONE', ( #307 ), #3291, .T. ) ;
#5555 = ORIENTED_EDGE ( 'NONE', *, *, #5034, .F. ) ;
#5556 = DIRECTION ( 'NONE',  ( -1.000000000000000000, 1.010728034814421376E-30, 1.090846720500930387E-30 ) ) ;
#5557 = CARTESIAN_POINT ( 'NONE',  ( 0.1999999999999987899, 0.000000000000000000, 0.000000000000000000 ) ) ;
#5558 = FACE_OUTER_BOUND ( 'NONE', #4309, .T. ) ;
#5559 = CARTESIAN_POINT ( 'NONE',  ( 3.054370817402615033E-30, -6.459281472512932609, 1.556709314830545976 ) ) ;
#5560 = CARTESIAN_POINT ( 'NONE',  ( -10.00000000000000178, 0.000000000000000000, 0.000000000000000000 ) ) ;
#5561 = VECTOR ( 'NONE', #5514, 1000.000000000000000 ) ;
#5562 = AXIS2_PLACEMENT_3D ( 'NONE', #5638, #8790, #12734 ) ;
#5563 = AXIS2_PLACEMENT_3D ( 'NONE', #11536, #8560, #7411 ) ;
#5564 = CARTESIAN_POINT ( 'NONE',  ( 0.000000000000000000, 0.000000000000000000, 0.000000000000000000 ) ) ;
#5565 = FILL_AREA_STYLE ('',( #3576 ) ) ;
#5566 = FACE_OUTER_BOUND ( 'NONE', #9035, .T. ) ;
#5567 = EDGE_LOOP ( 'NONE', ( #11623, #5831, #3703, #34, #6473, #2785, #4030 ) ) ;
#5568 = ORIENTED_EDGE ( 'NONE', *, *, #7279, .T. ) ;
#5569 = EDGE_CURVE ( 'NONE', #7175, #9454, #740, .T. ) ;
#5570 = ORIENTED_EDGE ( 'NONE', *, *, #564, .F. ) ;
#5571 = LINE ( 'NONE', #11242, #1505 ) ;
#5572 = EDGE_CURVE ( 'NONE', #4174, #8613, #11907, .T. ) ;
#5573 = CARTESIAN_POINT ( 'NONE',  ( 11.00000000000003020, 30.00000000000000000, 25.00000000000007105 ) ) ;
#5574 = CYLINDRICAL_SURFACE ( 'NONE', #11497, 4.000000000000000000 ) ;
#5575 = DIRECTION ( 'NONE',  ( -1.000000000000000000, 1.010728034814421376E-30, 1.090846720500930387E-30 ) ) ;
#5576 = ORIENTED_EDGE ( 'NONE', *, *, #12400, .T. ) ;
#5577 = CARTESIAN_POINT ( 'NONE',  ( 19.99999999999999645, 0.000000000000000000, 0.000000000000000000 ) ) ;
#5578 = ADVANCED_FACE ( 'NONE', ( #7141 ), #402, .F. ) ;
#5579 = ORIENTED_EDGE ( 'NONE', *, *, #11447, .F. ) ;
#5580 = EDGE_LOOP ( 'NONE', ( #9288, #9188, #10138, #2533 ) ) ;
#5581 = CARTESIAN_POINT ( 'NONE',  ( 2.000000000000007105, 3.464101615137750390, 6.938893903907228378E-15 ) ) ;
#5582 = ORIENTED_EDGE ( 'NONE', *, *, #11243, .F. ) ;
#5583 = ORIENTED_EDGE ( 'NONE', *, *, #9111, .T. ) ;
#5584 =( LENGTH_UNIT ( ) NAMED_UNIT ( * ) SI_UNIT ( .MILLI., .METRE. ) );
#5585 = FILL_AREA_STYLE ('',( #3599 ) ) ;
#5586 = ORIENTED_EDGE ( 'NONE', *, *, #8399, .T. ) ;
#5587 = DIRECTION ( 'NONE',  ( -1.000000000000000000, 0.000000000000000000, 0.000000000000000000 ) ) ;
#5588 = PLANE ( 'NONE',  #1414 ) ;
#5589 = VECTOR ( 'NONE', #6727, 1000.000000000000000 ) ;
#5590 = ORIENTED_EDGE ( 'NONE', *, *, #4940, .F. ) ;
#5591 = CARTESIAN_POINT ( 'NONE',  ( 19.99999999999999645, 0.000000000000000000, 0.000000000000000000 ) ) ;
#5592 = CARTESIAN_POINT ( 'NONE',  ( 27.00000000000000355, 21.47552320888931021, -7.222675303056225182 ) ) ;
#5593 = CYLINDRICAL_SURFACE ( 'NONE', #520, 2.800000000000003819 ) ;
#5594 = UNCERTAINTY_MEASURE_WITH_UNIT (LENGTH_MEASURE( 1.000000000000000082E-05 ), #2132, 'distance_accuracy_value', 'NONE');
#5595 = VECTOR ( 'NONE', #2001, 1000.000000000000000 ) ;
#5596 = ORIENTED_EDGE ( 'NONE', *, *, #6633, .F. ) ;
#5597 = AXIS2_PLACEMENT_3D ( 'NONE', #5749, #6791, #10511 ) ;
#5598 = ORIENTED_EDGE ( 'NONE', *, *, #9179, .F. ) ;
#5599 = DIRECTION ( 'NONE',  ( -1.158639454543359338E-30, 0.08963930890342672320, 0.9959742939952396235 ) ) ;
#5600 = DIRECTION ( 'NONE',  ( 3.143182988685428759E-16, -1.081682119347362623E-16, 1.000000000000000000 ) ) ;
#5601 = ORIENTED_EDGE ( 'NONE', *, *, #1145, .T. ) ;
#5602 = CYLINDRICAL_SURFACE ( 'NONE', #5563, 6.499000000000010324 ) ;
#5603 = FACE_BOUND ( 'NONE', #8737, .T. ) ;
#5604 = LINE ( 'NONE', #9267, #7302 ) ;
#5605 = CARTESIAN_POINT ( 'NONE',  ( 0.000000000000000000, 5.362412286431502473, -3.809543717993857381 ) ) ;
#5606 = ORIENTED_EDGE ( 'NONE', *, *, #5762, .T. ) ;
#5607 = CARTESIAN_POINT ( 'NONE',  ( -15.00000000000000000, 2.465190328815661892E-29, 20.00000000000007461 ) ) ;
#5608 = ORIENTED_EDGE ( 'NONE', *, *, #714, .F. ) ;
#5609 = AXIS2_PLACEMENT_3D ( 'NONE', #5359, #652, #6592 ) ;
#5610 = DIRECTION ( 'NONE',  ( -1.000000000000000000, 0.000000000000000000, 0.000000000000000000 ) ) ;
#5611 = VECTOR ( 'NONE', #5081, 1000.000000000000000 ) ;
#5612 = FILL_AREA_STYLE ('',( #3813 ) ) ;
#5613 = CARTESIAN_POINT ( 'NONE',  ( 19.99999999999997868, 6.496448636052932990, 0.1820882179769736653 ) ) ;
#5614 = CARTESIAN_POINT ( 'NONE',  ( 0.000000000000000000, 2.180689217871957908, -6.122221454264557217 ) ) ;
#5615 = DIRECTION ( 'NONE',  ( 0.000000000000000000, 1.000000000000000000, 0.000000000000000000 ) ) ;
#5616 = CARTESIAN_POINT ( 'NONE',  ( 40.00000000000000711, 20.75061298173632451, -7.028257169185711639 ) ) ;
#5617 = CARTESIAN_POINT ( 'NONE',  ( -30.00000000000000000, 19.99999999999999645, 1.734723475976807094E-15 ) ) ;
#5618 = CARTESIAN_POINT ( 'NONE',  ( 11.00000000000003730, -19.99999999999999645, 14.15000000000002345 ) ) ;
#5619 = CARTESIAN_POINT ( 'NONE',  ( 19.99999999999999645, -5.610543508060446882, 3.433640984893234549 ) ) ;
#5620 = EDGE_CURVE ( 'NONE', #937, #349, #2046, .T. ) ;
#5621 = EDGE_CURVE ( 'NONE', #5369, #4507, #6296, .T. ) ;
#5622 = LINE ( 'NONE', #725, #4103 ) ;
#5623 = EDGE_CURVE ( 'NONE', #12693, #5204, #5266, .T. ) ;
#5624 = ORIENTED_EDGE ( 'NONE', *, *, #4503, .T. ) ;
#5625 = AXIS2_PLACEMENT_3D ( 'NONE', #273, #11030, #5174 ) ;
#5626 = ORIENTED_EDGE ( 'NONE', *, *, #11802, .T. ) ;
#5627 = ORIENTED_EDGE ( 'NONE', *, *, #11487, .F. ) ;
#5628 = DIRECTION ( 'NONE',  ( -1.000000000000000000, 1.010728034814421376E-30, 1.090846720500930387E-30 ) ) ;
#5629 = DIRECTION ( 'NONE',  ( -1.429810390713081445E-30, 0.5877852522924684742, 0.8090169943749507819 ) ) ;
#5630 = PLANE ( 'NONE',  #171 ) ;
#5631 = CARTESIAN_POINT ( 'NONE',  ( 40.00000000000000711, 40.41548023366552655, -10.14535464186970692 ) ) ;
#5632 = ORIENTED_EDGE ( 'NONE', *, *, #11568, .T. ) ;
#5633 = FACE_OUTER_BOUND ( 'NONE', #6455, .T. ) ;
#5634 = TOROIDAL_SURFACE ( 'NONE', #281, 3.299999999999999822, 0.2000000000000000111 ) ;
#5635 = DIRECTION ( 'NONE',  ( -1.000000000000000000, 1.010728034814421376E-30, 1.090846720500930387E-30 ) ) ;
#5636 = ORIENTED_EDGE ( 'NONE', *, *, #5884, .T. ) ;
#5637 = ORIENTED_EDGE ( 'NONE', *, *, #2687, .T. ) ;
#5638 = CARTESIAN_POINT ( 'NONE',  ( 19.99999999999999645, 0.000000000000000000, 0.000000000000000000 ) ) ;
#5639 = VERTEX_POINT ( 'NONE', #5143 ) ;
#5640 = ORIENTED_EDGE ( 'NONE', *, *, #12514, .T. ) ;
#5641 = VECTOR ( 'NONE', #5430, 1000.000000000000000 ) ;
#5642 = CARTESIAN_POINT ( 'NONE',  ( 0.000000000000000000, -0.8865213383406691516, 1.535500000000002085 ) ) ;
#5643 = LINE ( 'NONE', #9557, #4938 ) ;
#5644 = ORIENTED_EDGE ( 'NONE', *, *, #1006, .F. ) ;
#5645 = DIRECTION ( 'NONE',  ( 1.000000000000000000, -0.000000000000000000, -6.938893903907228378E-17 ) ) ;
#5646 = EDGE_CURVE ( 'NONE', #6729, #11498, #9769, .T. ) ;
#5647 = DIRECTION ( 'NONE',  ( 3.260214209858708648E-30, 0.5000000000000012212, 0.8660254037844379305 ) ) ;
#5648 = ORIENTED_EDGE ( 'NONE', *, *, #333, .F. ) ;
#5649 = DIRECTION ( 'NONE',  ( 0.000000000000000000, 0.000000000000000000, 1.000000000000000000 ) ) ;
#5650 = LINE ( 'NONE', #9434, #5853 ) ;
#5651 = VECTOR ( 'NONE', #11134, 1000.000000000000000 ) ;
#5652 = EDGE_CURVE ( 'NONE', #6793, #7062, #4654, .T. ) ;
#5653 = ADVANCED_FACE ( 'NONE', ( #4173, #4297 ), #6167, .T. ) ;
#5654 = VERTEX_POINT ( 'NONE', #3098 ) ;
#5655 = VERTEX_POINT ( 'NONE', #12173 ) ;
#5656 = DIRECTION ( 'NONE',  ( 0.000000000000000000, 0.000000000000000000, 1.000000000000000000 ) ) ;
#5657 = DIRECTION ( 'NONE',  ( -1.000000000000000000, 1.821400096655618627E-30, 6.938893903906928857E-17 ) ) ;
#5658 = ORIENTED_EDGE ( 'NONE', *, *, #9957, .T. ) ;
#5659 = AXIS2_PLACEMENT_3D ( 'NONE', #7893, #3030, #10920 ) ;
#5660 = DIRECTION ( 'NONE',  ( 1.000000000000000000, 1.081682119347366197E-16, -6.938893903907228378E-17 ) ) ;
#5661 = CARTESIAN_POINT ( 'NONE',  ( -17.00000000000002842, 19.99999999999998579, 14.15000000000003055 ) ) ;
#5662 = CARTESIAN_POINT ( 'NONE',  ( -4.203833317240843748, -1.627343821129598966, -3.597273115243905028 ) ) ;
#5663 = EDGE_CURVE ( 'NONE', #7136, #7453, #11453, .T. ) ;
#5664 = AXIS2_PLACEMENT_3D ( 'NONE', #6399, #1691, #9592 ) ;
#5665 = CARTESIAN_POINT ( 'NONE',  ( 2.000000000000001776, 0.000000000000000000, 0.000000000000000000 ) ) ;
#5666 = ORIENTED_EDGE ( 'NONE', *, *, #7312, .F. ) ;
#5667 =( BOUNDED_SURFACE ( )  B_SPLINE_SURFACE ( 3, 2, ( 
 ( #11151, #389, #6251 ),
 ( #1544, #10156, #1482 ),
 ( #518, #4449, #8374 ),
 ( #1269, #8995, #7210 ),
 ( #5206, #10015, #177 ),
 ( #9123, #7016, #9889 ) ),
 .UNSPECIFIED., .F., .F., .T. ) 
 B_SPLINE_SURFACE_WITH_KNOTS ( ( 4, 2, 4 ),
 ( 3, 3 ),
 ( 0.02027065861071770947, 0.02273072267836921331, 0.02519078674602071716 ),
 ( 0.000000000000000000, 1.000000000000000000 ),
 .UNSPECIFIED. ) 
 GEOMETRIC_REPRESENTATION_ITEM ( )  RATIONAL_B_SPLINE_SURFACE ( (
 ( 1.000000000000000000, 0.8047781708337300444, 1.000000000000000000),
 ( 1.000000000000000000, 0.8123765190704228534, 1.000000000000000000),
 ( 1.000000000000000000, 0.8190656277165397903, 1.000000000000000000),
 ( 1.000000000000000000, 0.8192366903510730491, 1.000000000000000000),
 ( 1.000000000000000000, 0.8126138454303962755, 1.000000000000000000),
 ( 1.000000000000000000, 0.8047712246031432093, 1.000000000000000000) ) ) 
 REPRESENTATION_ITEM ( '' )  SURFACE ( )  );
#5668 = CYLINDRICAL_SURFACE ( 'NONE', #12361, 6.499000000000010324 ) ;
#5669 = ORIENTED_EDGE ( 'NONE', *, *, #3470, .F. ) ;
#5670 = DIRECTION ( 'NONE',  ( -1.000000000000000000, 1.010728034814421376E-30, 1.090846720500930387E-30 ) ) ;
#5671 =( LENGTH_UNIT ( ) NAMED_UNIT ( * ) SI_UNIT ( .MILLI., .METRE. ) );
#5672 = EDGE_CURVE ( 'NONE', #9760, #938, #1462, .T. ) ;
#5673 = CARTESIAN_POINT ( 'NONE',  ( 0.000000000000000000, 6.496448636052942760, 0.1820882179769667264 ) ) ;
#5674 = APPLICATION_CONTEXT ( 'automotive_design' ) ;
#5675 = DIRECTION ( 'NONE',  ( -1.000000000000000000, 0.000000000000000000, 0.000000000000000000 ) ) ;
#5676 = CARTESIAN_POINT ( 'NONE',  ( 0.000000000000000000, 1.764426149628233853, -7.186570834724189005 ) ) ;
#5677 = DIRECTION ( 'NONE',  ( -1.848892746611746419E-31, -1.000000000000000000, 3.250006781153460502E-32 ) ) ;
#5678 = CARTESIAN_POINT ( 'NONE',  ( -7.299729015828635442E-15, -4.736529461166059995, -3.681130640444390867 ) ) ;
#5679 = DIRECTION ( 'NONE',  ( -1.000000000000000000, 1.010728034814421376E-30, 1.090846720500930387E-30 ) ) ;
#5680 = DIRECTION ( 'NONE',  ( 0.000000000000000000, 0.000000000000000000, 1.000000000000000000 ) ) ;
#5681 = DIRECTION ( 'NONE',  ( 0.000000000000000000, 5.551115123125776539E-17, 1.000000000000000000 ) ) ;
#5682 = UNCERTAINTY_MEASURE_WITH_UNIT (LENGTH_MEASURE( 1.000000000000000082E-05 ), #5312, 'distance_accuracy_value', 'NONE');
#5683 = CIRCLE ( 'NONE', #7938, 2.800000000000002487 ) ;
#5684 = ADVANCED_FACE ( 'NONE', ( #684 ), #9368, .T. ) ;
#5685 = AXIS2_PLACEMENT_3D ( 'NONE', #2428, #9292, #8590 ) ;
#5686 = CARTESIAN_POINT ( 'NONE',  ( 0.000000000000000000, -30.00000000000000000, -7.999999999999998224 ) ) ;
#5687 = EDGE_LOOP ( 'NONE', ( #3062, #5576, #4930, #3427 ) ) ;
#5688 = VERTEX_POINT ( 'NONE', #4563 ) ;
#5689 = ORIENTED_EDGE ( 'NONE', *, *, #5372, .F. ) ;
#5690 = ADVANCED_FACE ( 'NONE', ( #9307, #2506, #4495 ), #496, .T. ) ;
#5691 = DIRECTION ( 'NONE',  ( 0.000000000000000000, 1.000000000000000000, 0.000000000000000000 ) ) ;
#5692 = CARTESIAN_POINT ( 'NONE',  ( -35.00000000000006395, -2.157041537713704155E-29, 2.000000000000003553 ) ) ;
#5694 = EDGE_CURVE ( 'NONE', #2020, #7959, #9494, .T. ) ;
#5693 = FACE_OUTER_BOUND ( 'NONE', #5438, .T. ) ;
#5695 = VECTOR ( 'NONE', #8769, 1000.000000000000000 ) ;
#5696 = CARTESIAN_POINT ( 'NONE',  ( 2.000000000000001776, 1.773042676681338303, 0.000000000000000000 ) ) ;
#5697 = ORIENTED_EDGE ( 'NONE', *, *, #4940, .T. ) ;
#5698 = VECTOR ( 'NONE', #5927, 1000.000000000000000 ) ;
#5699 = DIRECTION ( 'NONE',  ( -4.563833282352349791E-17, 0.000000000000000000, -1.000000000000000000 ) ) ;
#5700 = CARTESIAN_POINT ( 'NONE',  ( -10.00000000000000178, 0.000000000000000000, 0.000000000000000000 ) ) ;
#5701 = ORIENTED_EDGE ( 'NONE', *, *, #2000, .T. ) ;
#5702 = VERTEX_POINT ( 'NONE', #11326 ) ;
#5703 = DIRECTION ( 'NONE',  ( -1.000000000000000000, 1.010728034814421376E-30, 1.090846720500930387E-30 ) ) ;
#5704 = ORIENTED_EDGE ( 'NONE', *, *, #9415, .F. ) ;
#5705 = MANIFOLD_SOLID_BREP ( 'M4 Clearance Hole1', #6643 ) ;
#5706 = ORIENTED_EDGE ( 'NONE', *, *, #8700, .F. ) ;
#5707 = CARTESIAN_POINT ( 'NONE',  ( 0.000000000000000000, 0.000000000000000000, 0.000000000000000000 ) ) ;
#5708 = AXIS2_PLACEMENT_3D ( 'NONE', #9814, #10725, #9751 ) ;
#5709 = LINE ( 'NONE', #9616, #5545 ) ;
#5710 = ORIENTED_EDGE ( 'NONE', *, *, #7203, .F. ) ;
#5711 = DIRECTION ( 'NONE',  ( -3.437775699846489820E-17, -0.2951046417778627751, -0.9554649393887560960 ) ) ;
#5712 = LINE ( 'NONE', #11643, #11412 ) ;
#5713 = ORIENTED_EDGE ( 'NONE', *, *, #8690, .F. ) ;
#5714 = EDGE_CURVE ( 'NONE', #12227, #11665, #7395, .T. ) ;
#5715 = DIRECTION ( 'NONE',  ( 1.031682152609352680E-29, 1.000000000000000000, -1.498801083243958569E-15 ) ) ;
#5716 = DIRECTION ( 'NONE',  ( -1.000000000000000000, 1.010728034814421376E-30, 1.090846720500930387E-30 ) ) ;
#5717 = VERTEX_POINT ( 'NONE', #4364 ) ;
#5718 = ORIENTED_EDGE ( 'NONE', *, *, #1864, .T. ) ;
#5719 = LINE ( 'NONE', #9630, #10320 ) ;
#5720 = DIRECTION ( 'NONE',  ( 3.143182988685428759E-16, -1.081682119347362623E-16, 1.000000000000000000 ) ) ;
#5721 = EDGE_LOOP ( 'NONE', ( #7456, #4978, #7459, #9414 ) ) ;
#5722 = DIRECTION ( 'NONE',  ( 2.218671295934093250E-30, -5.551115123125776539E-17, -1.000000000000000000 ) ) ;
#5723 = AXIS2_PLACEMENT_3D ( 'NONE', #9477, #12603, #4482 ) ;
#5724 = MANIFOLD_SOLID_BREP ( 'Hex', #8272 ) ;
#5725 = ADVANCED_FACE ( 'NONE', ( #6340 ), #1449, .F. ) ;
#5726 = DIRECTION ( 'NONE',  ( 1.000000000000000000, -0.000000000000000000, -6.938893903907228378E-17 ) ) ;
#5727 = EDGE_CURVE ( 'NONE', #8539, #11730, #10129, .T. ) ;
#5728 = DIRECTION ( 'NONE',  ( -0.000000000000000000, -1.000000000000000000, 0.000000000000000000 ) ) ;
#5729 = CARTESIAN_POINT ( 'NONE',  ( 14.00000000000000000, 13.00000000000000000, -6.000000000000001776 ) ) ;
#5730 = ADVANCED_FACE ( 'NONE', ( #2368 ), #7259, .T. ) ;
#5731 = VERTEX_POINT ( 'NONE', #11054 ) ;
#5732 = AXIS2_PLACEMENT_3D ( 'NONE', #1890, #924, #12725 ) ;
#5733 = DIRECTION ( 'NONE',  ( -1.000000000000000000, 1.010728034814421376E-30, 1.090846720500930387E-30 ) ) ;
#5734 = ORIENTED_EDGE ( 'NONE', *, *, #6884, .F. ) ;
#5735 = DIRECTION ( 'NONE',  ( -1.848892746611746419E-31, -1.000000000000000000, 3.250006781153460502E-32 ) ) ;
#5736 = DIRECTION ( 'NONE',  ( 0.000000000000000000, -0.2951046417778627751, -0.9554649393887560960 ) ) ;
#5737 = AXIS2_PLACEMENT_3D ( 'NONE', #10756, #9845, #8889 ) ;
#5738 = CIRCLE ( 'NONE', #187, 10.00000000000000178 ) ;
#5739 = DIRECTION ( 'NONE',  ( 1.000000000000000000, -1.010728034814421376E-30, -1.090846720500930387E-30 ) ) ;
#5740 = CARTESIAN_POINT ( 'NONE',  ( 19.99999999999999645, -6.577476285968334224, 2.730038749994996294 ) ) ;
#5741 = AXIS2_PLACEMENT_3D ( 'NONE', #2837, #1969, #8799 ) ;
#5742 = FACE_OUTER_BOUND ( 'NONE', #933, .T. ) ;
#5743 = CARTESIAN_POINT ( 'NONE',  ( 40.00000000000000711, 11.10553687445043103, -10.07215277424222855 ) ) ;
#5744 = DIRECTION ( 'NONE',  ( 1.140150527077241873E-30, 0.000000000000000000, -1.000000000000000000 ) ) ;
#5745 = CARTESIAN_POINT ( 'NONE',  ( 19.99999999999999645, -6.289597356626510205, 3.898841506334512541 ) ) ;
#5746 = CARTESIAN_POINT ( 'NONE',  ( 2.000000000000001776, 0.000000000000000000, 0.000000000000000000 ) ) ;
#5747 = AXIS2_PLACEMENT_3D ( 'NONE', #3699, #11559, #11023 ) ;
#5748 = CIRCLE ( 'NONE', #611, 2.800000000000002931 ) ;
#5749 = CARTESIAN_POINT ( 'NONE',  ( 15.00000000000003375, -12.49999999999999645, 3.994800001834461867E-31 ) ) ;
#5750 = AXIS2_PLACEMENT_3D ( 'NONE', #6673, #1511, #10584 ) ;
#5751 = VERTEX_POINT ( 'NONE', #11179 ) ;
#5752 = ORIENTED_EDGE ( 'NONE', *, *, #8915, .F. ) ;
#5753 = DIRECTION ( 'NONE',  ( 1.000000000000000000, 1.081682119347366197E-16, -6.938893903907228378E-17 ) ) ;
#5754 = AXIS2_PLACEMENT_3D ( 'NONE', #6221, #10326, #1456 ) ;
#5755 = DIRECTION ( 'NONE',  ( 0.000000000000000000, 1.000000000000000000, 0.000000000000000000 ) ) ;
#5756 = AXIS2_PLACEMENT_3D ( 'NONE', #7533, #5539, #9573 ) ;
#5757 = CYLINDRICAL_SURFACE ( 'NONE', #6302, 2.149999999999999023 ) ;
#5758 = ORIENTED_EDGE ( 'NONE', *, *, #9989, .T. ) ;
#5759 = CARTESIAN_POINT ( 'NONE',  ( 2.000000000000001776, 1.773042676681341856, -3.469446951953614189E-15 ) ) ;
#5760 = EDGE_LOOP ( 'NONE', ( #5010, #7794, #10068, #7968 ) ) ;
#5761 = ORIENTED_EDGE ( 'NONE', *, *, #12015, .T. ) ;
#5762 = EDGE_CURVE ( 'NONE', #6277, #5068, #11654, .T. ) ;
#5763 = PLANE ( 'NONE',  #5326 ) ;
#5764 = ORIENTED_EDGE ( 'NONE', *, *, #997, .F. ) ;
#5765 =( GEOMETRIC_REPRESENTATION_CONTEXT ( 3 ) GLOBAL_UNCERTAINTY_ASSIGNED_CONTEXT ( ( #11494 ) ) GLOBAL_UNIT_ASSIGNED_CONTEXT ( ( #1779, #12482, #5043 ) ) REPRESENTATION_CONTEXT ( 'NONE', 'WORKASPACE' ) );
#5766 = STYLED_ITEM ( 'NONE', ( #2019 ), #10029 ) ;
#5767 = ORIENTED_EDGE ( 'NONE', *, *, #3203, .T. ) ;
#5768 = DIRECTION ( 'NONE',  ( 0.000000000000000000, 0.000000000000000000, 1.000000000000000000 ) ) ;
#5769 = ORIENTED_EDGE ( 'NONE', *, *, #4486, .T. ) ;
#5770 = DIRECTION ( 'NONE',  ( -1.000000000000000000, 1.010728034814421376E-30, 1.090846720500930387E-30 ) ) ;
#5771 = DIRECTION ( 'NONE',  ( 0.000000000000000000, 0.000000000000000000, 1.000000000000000000 ) ) ;
#5772 = EDGE_LOOP ( 'NONE', ( #2511, #5352, #4890, #8618, #7669 ) ) ;
#5773 = LINE ( 'NONE', #11838, #5507 ) ;
#5774 = DIRECTION ( 'NONE',  ( -0.000000000000000000, -1.000000000000000000, 0.000000000000000000 ) ) ;
#5775 = ORIENTED_EDGE ( 'NONE', *, *, #2919, .F. ) ;
#5776 = ORIENTED_EDGE ( 'NONE', *, *, #1275, .F. ) ;
#5777 = ADVANCED_FACE ( 'NONE', ( #10252 ), #5376, .F. ) ;
#5778 = VERTEX_POINT ( 'NONE', #10069 ) ;
#5779 = CARTESIAN_POINT ( 'NONE',  ( -30.00000000000000000, 0.000000000000000000, 3.477184903947654954E-15 ) ) ;
#5780 = CIRCLE ( 'NONE', #9672, 10.00000000000000178 ) ;
#5781 = ORIENTED_EDGE ( 'NONE', *, *, #2687, .F. ) ;
#5782 = CARTESIAN_POINT ( 'NONE',  ( 2.000000000000007105, -3.464101615137750390, -1.734723475976807094E-14 ) ) ;
#5783 = ORIENTED_EDGE ( 'NONE', *, *, #4464, .F. ) ;
#5784 = MANIFOLD_SOLID_BREP ( 'Cut-Extrude1', #6004 ) ;
#5785 = DIRECTION ( 'NONE',  ( 1.000000000000000000, 5.916456789157575403E-31, -1.577021341797098546E-16 ) ) ;
#5786 = CIRCLE ( 'NONE', #6416, 6.499000000000011212 ) ;
#5787 = CARTESIAN_POINT ( 'NONE',  ( 3.999999999999996447, 0.000000000000000000, 0.000000000000000000 ) ) ;
#5788 = AXIS2_PLACEMENT_3D ( 'NONE', #9912, #267, #5876 ) ;
#5789 = EDGE_CURVE ( 'NONE', #4412, #9489, #12093, .T. ) ;
#5790 = DIRECTION ( 'NONE',  ( -1.000000000000000000, -5.916456789157575403E-31, 1.577021341797098793E-16 ) ) ;
#5791 = ORIENTED_EDGE ( 'NONE', *, *, #7038, .F. ) ;
#5792 = CARTESIAN_POINT ( 'NONE',  ( 19.99999999999999645, -6.459281472512932609, -1.243290685169442966 ) ) ;
#5793 = EDGE_LOOP ( 'NONE', ( #6551, #9613, #413, #1124 ) ) ;
#5794 = EDGE_CURVE ( 'NONE', #2957, #8146, #8160, .T. ) ;
#5795 = CARTESIAN_POINT ( 'NONE',  ( -11.83215956619923226, 30.00000000000000000, 2.000000000000000000 ) ) ;
#5796 = EDGE_CURVE ( 'NONE', #4162, #4793, #3850, .T. ) ;
#5797 = CYLINDRICAL_SURFACE ( 'NONE', #6599, 6.499000000000010324 ) ;
#5798 = CIRCLE ( 'NONE', #2529, 2.149999999999999023 ) ;
#5799 = CARTESIAN_POINT ( 'NONE',  ( 0.000000000000000000, 7.100173756228453037, -2.085073771204482007 ) ) ;
#5800 = EDGE_CURVE ( 'NONE', #2961, #2884, #3249, .T. ) ;
#5801 = DIRECTION ( 'NONE',  ( 0.000000000000000000, 0.000000000000000000, -1.000000000000000000 ) ) ;
#5802 = DIRECTION ( 'NONE',  ( -1.000000000000000000, 1.010728034814421376E-30, 1.090846720500930387E-30 ) ) ;
#5803 = FACE_OUTER_BOUND ( 'NONE', #1517, .T. ) ;
#5804 = LINE ( 'NONE', #2870, #2601 ) ;
#5805 = CARTESIAN_POINT ( 'NONE',  ( -17.00000000000002842, 19.99999999999998579, 12.00000000000003730 ) ) ;
#5806 = CIRCLE ( 'NONE', #256, 2.499999999999998668 ) ;
#5807 = VECTOR ( 'NONE', #10421, 1000.000000000000000 ) ;
#5808 = CARTESIAN_POINT ( 'NONE',  ( 2.000000000000007105, -3.464101615137750390, -1.734723475976807094E-14 ) ) ;
#5809 = ADVANCED_FACE ( 'NONE', ( #3338 ), #10186, .T. ) ;
#5810 = DIRECTION ( 'NONE',  ( 0.000000000000000000, 0.000000000000000000, -1.000000000000000000 ) ) ;
#5811 = EDGE_CURVE ( 'NONE', #93, #1090, #12220, .T. ) ;
#5812 = ORIENTED_EDGE ( 'NONE', *, *, #646, .T. ) ;
#5813 = ORIENTED_EDGE ( 'NONE', *, *, #10492, .T. ) ;
#5814 = CIRCLE ( 'NONE', #2088, 2.149999999999999023 ) ;
#5815 = DIRECTION ( 'NONE',  ( -1.000000000000000000, 0.000000000000000000, 0.000000000000000000 ) ) ;
#5816 = CIRCLE ( 'NONE', #1292, 2.000000000000000888 ) ;
#5817 = DIRECTION ( 'NONE',  ( 0.000000000000000000, 4.478906847412178337E-32, -1.000000000000000000 ) ) ;
#5818 = CARTESIAN_POINT ( 'NONE',  ( 5.560781378645591744, -2.788447640341963522E-15, -4.000000000000010658 ) ) ;
#5819 = CARTESIAN_POINT ( 'NONE',  ( 19.99999999999997868, 3.975087478966734533, -6.241688836730180157 ) ) ;
#5820 = ORIENTED_EDGE ( 'NONE', *, *, #5960, .F. ) ;
#5821 = DIRECTION ( 'NONE',  ( 0.000000000000000000, 0.9195277725514489076, 0.3930250316539278255 ) ) ;
#5822 = EDGE_CURVE ( 'NONE', #5862, #4933, #11457, .T. ) ;
#5823 = CARTESIAN_POINT ( 'NONE',  ( 0.000000000000000000, 5.670261409740643188, 3.175710400084689411 ) ) ;
#5824 = EDGE_CURVE ( 'NONE', #9207, #1632, #12287, .T. ) ;
#5825 = DIRECTION ( 'NONE',  ( 0.000000000000000000, 0.000000000000000000, -1.000000000000000000 ) ) ;
#5826 = ORIENTED_EDGE ( 'NONE', *, *, #3622, .F. ) ;
#5827 = VECTOR ( 'NONE', #3261, 1000.000000000000000 ) ;
#5828 = ORIENTED_EDGE ( 'NONE', *, *, #1553, .F. ) ;
#5829 = PLANE ( 'NONE',  #1413 ) ;
#5830 = ORIENTED_EDGE ( 'NONE', *, *, #6965, .F. ) ;
#5831 = ORIENTED_EDGE ( 'NONE', *, *, #6988, .T. ) ;
#5832 = EDGE_CURVE ( 'NONE', #1077, #10196, #4669, .T. ) ;
#5833 = CARTESIAN_POINT ( 'NONE',  ( -2.000000000000008882, -3.464101615137750390, -8.673617379884035472E-15 ) ) ;
#5834 = ORIENTED_EDGE ( 'NONE', *, *, #5988, .T. ) ;
#5835 = CARTESIAN_POINT ( 'NONE',  ( 1.734723475976807094E-14, -3.469446951953614189E-15, -4.000000000000010658 ) ) ;
#5836 = ADVANCED_FACE ( 'NONE', ( #3585 ), #4247, .T. ) ;
#5837 = LINE ( 'NONE', #9560, #7472 ) ;
#5838 = ORIENTED_EDGE ( 'NONE', *, *, #9824, .T. ) ;
#5839 = AXIS2_PLACEMENT_3D ( 'NONE', #9654, #8708, #10691 ) ;
#5840 = DIRECTION ( 'NONE',  ( 0.000000000000000000, 0.000000000000000000, 1.000000000000000000 ) ) ;
#5841 = CARTESIAN_POINT ( 'NONE',  ( 20.00000000000000355, 20.75061298173632096, -7.028257169185711639 ) ) ;
#5842 = CIRCLE ( 'NONE', #8726, 5.000000000000000888 ) ;
#5843 = ORIENTED_EDGE ( 'NONE', *, *, #7676, .F. ) ;
#5844 = EDGE_LOOP ( 'NONE', ( #103, #12223, #5791, #4120 ) ) ;
#5845 = CIRCLE ( 'NONE', #292, 2.499999999999998668 ) ;
#5846 = VERTEX_POINT ( 'NONE', #11307 ) ;
#5847 = EDGE_CURVE ( 'NONE', #175, #3101, #3036, .T. ) ;
#5848 = LINE ( 'NONE', #1143, #5611 ) ;
#5849 = ORIENTED_EDGE ( 'NONE', *, *, #8477, .F. ) ;
#5850 = CARTESIAN_POINT ( 'NONE',  ( 9.999999999999998224, 7.100173756228454813, -2.085073771204489113 ) ) ;
#5851 = ORIENTED_EDGE ( 'NONE', *, *, #11926, .F. ) ;
#5852 = AXIS2_PLACEMENT_3D ( 'NONE', #1289, #11994, #3118 ) ;
#5853 = VECTOR ( 'NONE', #3606, 1000.000000000000000 ) ;
#5854 = LINE ( 'NONE', #8624, #398 ) ;
#5855 = EDGE_CURVE ( 'NONE', #5655, #229, #133, .T. ) ;
#5856 = EDGE_CURVE ( 'NONE', #9808, #1261, #10192, .T. ) ;
#5857 = DIRECTION ( 'NONE',  ( -1.000000000000000000, 1.006188713385347367E-17, 3.844790828812615713E-17 ) ) ;
#5858 = DIRECTION ( 'NONE',  ( -1.140150527077241873E-30, 0.000000000000000000, 1.000000000000000000 ) ) ;
#5859 = VERTEX_POINT ( 'NONE', #2554 ) ;
#5860 = CARTESIAN_POINT ( 'NONE',  ( -10.00000000000000178, 0.000000000000000000, 0.000000000000000000 ) ) ;
#5861 = CIRCLE ( 'NONE', #4638, 6.499000000000010324 ) ;
#5862 = VERTEX_POINT ( 'NONE', #9601 ) ;
#5863 = AXIS2_PLACEMENT_3D ( 'NONE', #5887, #4923, #1955 ) ;
#5864 = CARTESIAN_POINT ( 'NONE',  ( 19.99999999999999645, 3.975087478966644383, 6.241688836730229006 ) ) ;
#5865 = DIRECTION ( 'NONE',  ( 0.000000000000000000, 0.8345732537213000901, 0.5508969814521065267 ) ) ;
#5866 = B_SPLINE_CURVE_WITH_KNOTS ( 'NONE', 3,
 ( #8450, #6326, #10374, #5363, #9280, #6263 ),
 .UNSPECIFIED., .F., .F.,
 ( 4, 2, 4 ),
 ( 0.000000000000000000, 0.0002095117440864779055, 0.0004190234881729558111 ),
 .UNSPECIFIED. ) ;
#5867 = DIRECTION ( 'NONE',  ( -1.000000000000000000, 1.010728034814421376E-30, 1.090846720500930387E-30 ) ) ;
#5868 = DIRECTION ( 'NONE',  ( 1.000000000000000000, -1.010728034814421376E-30, -1.090846720500930387E-30 ) ) ;
#5869 = EDGE_CURVE ( 'NONE', #7720, #11206, #10418, .T. ) ;
#5870 = CARTESIAN_POINT ( 'NONE',  ( 19.99999999999999645, -4.155687294075622873, 5.098857909653524700 ) ) ;
#5871 = CIRCLE ( 'NONE', #4443, 6.499000000000011212 ) ;
#5872 = DIRECTION ( 'NONE',  ( 0.000000000000000000, 0.000000000000000000, -1.000000000000000000 ) ) ;
#5873 = CARTESIAN_POINT ( 'NONE',  ( 27.00000000000000355, 39.34792583643766051, -17.06347054209567915 ) ) ;
#5874 = DIRECTION ( 'NONE',  ( 1.000000000000000000, -1.010728034814421376E-30, -1.090846720500930387E-30 ) ) ;
#5875 = EDGE_CURVE ( 'NONE', #3108, #4020, #7140, .T. ) ;
#5876 = DIRECTION ( 'NONE',  ( 1.405158487424925001E-30, -0.3513748240813304724, -0.9362348706397417564 ) ) ;
#5877 = VECTOR ( 'NONE', #201, 1000.000000000000114 ) ;
#5878 = PRESENTATION_LAYER_ASSIGNMENT (  '', '', ( #2611 ) ) ;
#5879 = VERTEX_POINT ( 'NONE', #10388 ) ;
#5880 = DIRECTION ( 'NONE',  ( -1.000000000000000000, 1.010728034814421376E-30, 1.090846720500930387E-30 ) ) ;
#5881 = DIRECTION ( 'NONE',  ( 0.000000000000000000, 0.000000000000000000, 1.000000000000000000 ) ) ;
#5882 = DIRECTION ( 'NONE',  ( 1.031065855027149465E-29, 1.000000000000000000, -7.771561172376086908E-16 ) ) ;
#5883 = DIRECTION ( 'NONE',  ( 0.000000000000000000, 1.000000000000000000, 0.000000000000000000 ) ) ;
#5884 = EDGE_CURVE ( 'NONE', #802, #6992, #608, .T. ) ;
#5885 = CARTESIAN_POINT ( 'NONE',  ( -18.00000000000002842, -30.00000000000000000, 1.369224906555730040E-16 ) ) ;
#5886 = ORIENTED_EDGE ( 'NONE', *, *, #3155, .T. ) ;
#5887 = CARTESIAN_POINT ( 'NONE',  ( 19.99999999999997868, 6.557268578288205418, -0.5199208220221240850 ) ) ;
#5888 = EDGE_CURVE ( 'NONE', #3594, #5515, #7940, .T. ) ;
#5889 = AXIS2_PLACEMENT_3D ( 'NONE', #7381, #12350, #9413 ) ;
#5890 = DIRECTION ( 'NONE',  ( 0.000000000000000000, 1.000000000000000000, -1.467581828789149335E-15 ) ) ;
#5891 = COLOUR_RGB ( '', 0.08235294, 0.09019608, 0.10196078) ;
#5892 = CARTESIAN_POINT ( 'NONE',  ( 2.000000000000001776, -1.329782007511014275, 0.7677500000000114788 ) ) ;
#5893 = ORIENTED_EDGE ( 'NONE', *, *, #3470, .T. ) ;
#5894 = VERTEX_POINT ( 'NONE', #4609 ) ;
#5895 = DIRECTION ( 'NONE',  ( -1.081682119347366321E-16, 1.000000000000000000, 0.000000000000000000 ) ) ;
#5896 = ORIENTED_EDGE ( 'NONE', *, *, #9076, .T. ) ;
#5897 = EDGE_LOOP ( 'NONE', ( #8733, #11176, #1079 ) ) ;
#5898 = CARTESIAN_POINT ( 'NONE',  ( 14.00000000000000000, -30.00000000000000000, 0.000000000000000000 ) ) ;
#5899 = ORIENTED_EDGE ( 'NONE', *, *, #3893, .F. ) ;
#5900 = VECTOR ( 'NONE', #6532, 1000.000000000000000 ) ;
#5901 = CARTESIAN_POINT ( 'NONE',  ( 19.99999999999999645, 0.000000000000000000, 0.000000000000000000 ) ) ;
#5902 = CYLINDRICAL_SURFACE ( 'NONE', #6471, 2.800000000000003819 ) ;
#5903 = ORIENTED_EDGE ( 'NONE', *, *, #12657, .F. ) ;
#5904 = CARTESIAN_POINT ( 'NONE',  ( 19.99999999999997868, -0.8135880386782390339, -6.527339685683426929 ) ) ;
#5905 = CARTESIAN_POINT ( 'NONE',  ( 0.000000000000000000, 5.670261409740692038, -3.175710400084609475 ) ) ;
#5906 = AXIS2_PLACEMENT_3D ( 'NONE', #10884, #5036, #2993 ) ;
#5907 = VERTEX_POINT ( 'NONE', #12346 ) ;
#5908 = CIRCLE ( 'NONE', #10824, 6.499000000000009436 ) ;
#5909 = EDGE_CURVE ( 'NONE', #47, #509, #2408, .T. ) ;
#5910 = ORIENTED_EDGE ( 'NONE', *, *, #896, .F. ) ;
#5911 = ORIENTED_EDGE ( 'NONE', *, *, #2301, .F. ) ;
#5912 = CARTESIAN_POINT ( 'NONE',  ( 19.99999999999999645, 0.000000000000000000, 0.000000000000000000 ) ) ;
#5913 = ORIENTED_EDGE ( 'NONE', *, *, #120, .F. ) ;
#5914 = LINE ( 'NONE', #12632, #8199 ) ;
#5915 = ORIENTED_EDGE ( 'NONE', *, *, #4077, .F. ) ;
#5916 = FACE_OUTER_BOUND ( 'NONE', #1971, .T. ) ;
#5917 = CARTESIAN_POINT ( 'NONE',  ( 19.99999999999999645, -5.148708580507705967, 3.965829163366258570 ) ) ;
#5918 = APPLICATION_CONTEXT ( 'automotive_design' ) ;
#5919 = VERTEX_POINT ( 'NONE', #9541 ) ;
#5920 = DIRECTION ( 'NONE',  ( -1.000000000000000000, 1.010728034814421376E-30, 1.090846720500930387E-30 ) ) ;
#5921 = ORIENTED_EDGE ( 'NONE', *, *, #9304, .F. ) ;
#5922 = DIRECTION ( 'NONE',  ( -1.000000000000000000, 1.010728034814421376E-30, 1.090846720500930387E-30 ) ) ;
#5923 = EDGE_CURVE ( 'NONE', #9663, #1734, #6930, .T. ) ;
#5924 = EDGE_CURVE ( 'NONE', #11920, #12737, #4040, .T. ) ;
#5925 = DIRECTION ( 'NONE',  ( -1.000000000000000000, 6.162975822039154730E-33, 4.563833282352349791E-17 ) ) ;
#5926 = DIRECTION ( 'NONE',  ( 0.000000000000000000, -1.530455820933490821E-32, 1.000000000000000000 ) ) ;
#5927 = DIRECTION ( 'NONE',  ( -1.000000000000000000, -5.916456789157575403E-31, -2.465190328815656418E-32 ) ) ;
#5928 = CARTESIAN_POINT ( 'NONE',  ( 19.99999999999999645, -6.133480037816472219, -2.376659734729558160 ) ) ;
#5929 = CYLINDRICAL_SURFACE ( 'NONE', #4004, 4.499999999999999112 ) ;
#5930 = AXIS2_PLACEMENT_3D ( 'NONE', #11816, #10832, #4014 ) ;
#5931 = CARTESIAN_POINT ( 'NONE',  ( 15.00000000000003375, 12.50000000000000000, -6.000000000000000000 ) ) ;
#5932 = CARTESIAN_POINT ( 'NONE',  ( 0.000000000000000000, 4.596015818000147135, -4.705818469689461381 ) ) ;
#5933 = LINE ( 'NONE', #9851, #10525 ) ;
#5934 = ADVANCED_FACE ( 'NONE', ( #8526 ), #12470, .F. ) ;
#5935 = AXIS2_PLACEMENT_3D ( 'NONE', #3931, #1088, #5027 ) ;
#5936 = AXIS2_PLACEMENT_3D ( 'NONE', #1798, #9634, #830 ) ;
#5937 = PRODUCT_DEFINITION ( 'UNKNOWN', '', #7948, #5154 ) ;
#5938 = COLOUR_RGB ( '', 0.66274510, 0.83137255, 0.94901961) ;
#5939 = ORIENTED_EDGE ( 'NONE', *, *, #507, .T. ) ;
#5940 = ORIENTED_EDGE ( 'NONE', *, *, #4969, .T. ) ;
#5941 = DIRECTION ( 'NONE',  ( 0.000000000000000000, 0.000000000000000000, 1.000000000000000000 ) ) ;
#5942 = PLANE ( 'NONE',  #4255 ) ;
#5943 = DIRECTION ( 'NONE',  ( -1.000000000000000000, 1.010728034814421376E-30, 1.090846720500930387E-30 ) ) ;
#5944 = FACE_OUTER_BOUND ( 'NONE', #10010, .T. ) ;
#5945 = ORIENTED_EDGE ( 'NONE', *, *, #12715, .F. ) ;
#5946 = DIRECTION ( 'NONE',  ( 0.000000000000000000, 0.000000000000000000, 1.000000000000000000 ) ) ;
#5947 = AXIS2_PLACEMENT_3D ( 'NONE', #1227, #202, #6191 ) ;
#5948 = FACE_BOUND ( 'NONE', #10452, .T. ) ;
#5949 = CARTESIAN_POINT ( 'NONE',  ( 19.99999999999999645, 0.000000000000000000, 0.000000000000000000 ) ) ;
#5950 = EDGE_LOOP ( 'NONE', ( #7629, #2240, #8747, #4359 ) ) ;
#5951 = CIRCLE ( 'NONE', #11931, 2.800000000000003375 ) ;
#5952 = EDGE_CURVE ( 'NONE', #302, #7500, #2839, .T. ) ;
#5953 = ORIENTED_EDGE ( 'NONE', *, *, #1477, .T. ) ;
#5954 = CARTESIAN_POINT ( 'NONE',  ( 5.603754474796030917E-15, 4.736522675502333080, -3.681124513963746292 ) ) ;
#5955 = ORIENTED_EDGE ( 'NONE', *, *, #5847, .F. ) ;
#5956 = MANIFOLD_SOLID_BREP ( 'Boss-Extrude1', #9901 ) ;
#5957 = ORIENTED_EDGE ( 'NONE', *, *, #9891, .F. ) ;
#5958 = APPLICATION_PROTOCOL_DEFINITION ( 'draft international standard', 'automotive_design', 1998, #2397 ) ;
#5959 = EDGE_CURVE ( 'NONE', #9310, #3242, #6413, .T. ) ;
#5960 = EDGE_CURVE ( 'NONE', #9234, #3660, #6103, .T. ) ;
#5961 = CIRCLE ( 'NONE', #4101, 2.800000000000002931 ) ;
#5962 = DIRECTION ( 'NONE',  ( -1.000000000000000000, 1.010728034814421376E-30, 1.090846720500930387E-30 ) ) ;
#5963 = AXIS2_PLACEMENT_3D ( 'NONE', #8893, #3058, #6973 ) ;
#5964 = ORIENTED_EDGE ( 'NONE', *, *, #8855, .F. ) ;
#5965 = VECTOR ( 'NONE', #2026, 1000.000000000000114 ) ;
#5966 = LINE ( 'NONE', #7257, #9914 ) ;
#5967 = ORIENTED_EDGE ( 'NONE', *, *, #2569, .F. ) ;
#5968 = DIRECTION ( 'NONE',  ( -1.000000000000000000, -1.031065855027150586E-29, 2.218671295934095703E-30 ) ) ;
#5969 = EDGE_CURVE ( 'NONE', #7775, #529, #11888, .T. ) ;
#5970 = DIRECTION ( 'NONE',  ( 0.000000000000000000, -0.08963930890344096181, 0.9959742939952382912 ) ) ;
#5971 = VECTOR ( 'NONE', #1410, 1000.000000000000000 ) ;
#5972 = ORIENTED_EDGE ( 'NONE', *, *, #65, .F. ) ;
#5973 = VERTEX_POINT ( 'NONE', #2880 ) ;
#5974 = ORIENTED_EDGE ( 'NONE', *, *, #3140, .T. ) ;
#5975 = DIRECTION ( 'NONE',  ( 0.000000000000000000, -0.6579387259397028176, -0.7530714660036194052 ) ) ;
#5976 = CARTESIAN_POINT ( 'NONE',  ( -3.453038570458820455, -2.625189405339339199, -3.535263753544679588 ) ) ;
#5977 = VERTEX_POINT ( 'NONE', #6860 ) ;
#5978 = DIRECTION ( 'NONE',  ( -1.000000000000000000, 1.010728034814421376E-30, 1.090846720500930387E-30 ) ) ;
#5979 =( GEOMETRIC_REPRESENTATION_CONTEXT ( 3 ) GLOBAL_UNCERTAINTY_ASSIGNED_CONTEXT ( ( #10346 ) ) GLOBAL_UNIT_ASSIGNED_CONTEXT ( ( #11284, #8444, #461 ) ) REPRESENTATION_CONTEXT ( 'NONE', 'WORKASPACE' ) );
#5980 = ORIENTED_EDGE ( 'NONE', *, *, #7545, .F. ) ;
#5981 = B_SPLINE_CURVE_WITH_KNOTS ( 'NONE', 3,
 ( #774, #7737, #11664, #4119, #8758, #3109 ),
 .UNSPECIFIED., .F., .F.,
 ( 4, 2, 4 ),
 ( 0.000000000000000000, 0.0002095117440864783663, 0.0004190234881729567326 ),
 .UNSPECIFIED. ) ;
#5982 = CARTESIAN_POINT ( 'NONE',  ( 33.00000000000001421, 81.84122341717352356, -2.681985084641642203 ) ) ;
#5983 = DIRECTION ( 'NONE',  ( -0.000000000000000000, -1.000000000000000000, -0.000000000000000000 ) ) ;
#5984 = ORIENTED_EDGE ( 'NONE', *, *, #5232, .F. ) ;
#5985 = CARTESIAN_POINT ( 'NONE',  ( 11.00000000000003375, -3.490243377569943242E-16, 22.15000000000002345 ) ) ;
#5986 = EDGE_LOOP ( 'NONE', ( #3285, #5752, #2081, #11496 ) ) ;
#5987 = DIRECTION ( 'NONE',  ( -1.000000000000000000, 1.010728034814421376E-30, 1.090846720500930387E-30 ) ) ;
#5988 = EDGE_CURVE ( 'NONE', #10595, #6024, #6923, .T. ) ;
#5989 = CARTESIAN_POINT ( 'NONE',  ( 20.00000000000000000, 8.901672616175321906, -15.56445005073997301 ) ) ;
#5990 = CARTESIAN_POINT ( 'NONE',  ( 27.00000000000000355, 30.14235464176399404, -24.26236220746664785 ) ) ;
#5991 = CIRCLE ( 'NONE', #1465, 2.800000000000002043 ) ;
#5992 = DIRECTION ( 'NONE',  ( 0.000000000000000000, 4.478906847412178337E-32, -1.000000000000000000 ) ) ;
#5993 = DIRECTION ( 'NONE',  ( -0.000000000000000000, -1.000000000000000000, -0.000000000000000000 ) ) ;
#5994 = DIRECTION ( 'NONE',  ( 1.000000000000000000, -6.162975822039154730E-33, -4.563833282352349791E-17 ) ) ;
#5995 = CARTESIAN_POINT ( 'NONE',  ( 14.00000000000000000, 30.00000000000000000, -6.000000000000000000 ) ) ;
#5996 = LINE ( 'NONE', #9911, #8426 ) ;
#5997 = DIRECTION ( 'NONE',  ( -1.000000000000000000, 1.010728034814421376E-30, 1.090846720500930387E-30 ) ) ;
#5998 = CIRCLE ( 'NONE', #452, 6.499000000000008548 ) ;
#5999 = EDGE_LOOP ( 'NONE', ( #10802, #7148 ) ) ;
#6000 = VERTEX_POINT ( 'NONE', #3951 ) ;
#6001 = DIRECTION ( 'NONE',  ( 2.206481006425900381E-16, -1.000000000000000000, 0.000000000000000000 ) ) ;
#6002 = LINE ( 'NONE', #9920, #8565 ) ;
#6003 = LINE ( 'NONE', #9667, #789 ) ;
#6004 = CLOSED_SHELL ( 'NONE', ( #12141, #3464, #1287, #532, #10260, #11773, #2810, #1127, #1000, #7536, #5053, #1049, #9283, #2878, #1048, #11690, #1083, #8159, #10444, #2843, #12195, #4526, #7920, #377, #7567, #2387, #8635, #11079, #12528, #1259, #12322, #7471 ) ) ;
#6005 = DIRECTION ( 'NONE',  ( 1.000000000000000000, -1.010728034814421376E-30, -1.090846720500930387E-30 ) ) ;
#6006 = ORIENTED_EDGE ( 'NONE', *, *, #1720, .F. ) ;
#6007 = EDGE_CURVE ( 'NONE', #8095, #6098, #6002, .T. ) ;
#6008 = CARTESIAN_POINT ( 'NONE',  ( 0.000000000000000000, 2.520781513113648398, 6.075668640744193105 ) ) ;
#6009 = AXIS2_PLACEMENT_3D ( 'NONE', #7028, #8820, #6842 ) ;
#6010 = ADVANCED_FACE ( 'NONE', ( #10704 ), #4982, .T. ) ;
#6011 = EDGE_CURVE ( 'NONE', #5079, #7729, #4855, .T. ) ;
#6012 = FACE_OUTER_BOUND ( 'NONE', #1172, .T. ) ;
#6013 = CARTESIAN_POINT ( 'NONE',  ( 2.000000000000001776, 1.773042676681338303, 0.000000000000000000 ) ) ;
#6014 = ORIENTED_EDGE ( 'NONE', *, *, #7796, .T. ) ;
#6015 = VERTEX_POINT ( 'NONE', #8721 ) ;
#6016 = CARTESIAN_POINT ( 'NONE',  ( 11.00000000000003730, -19.99999999999999645, 12.00000000000003553 ) ) ;
#6017 = EDGE_LOOP ( 'NONE', ( #5373, #5598, #287, #346 ) ) ;
#6018 = ORIENTED_EDGE ( 'NONE', *, *, #120, .T. ) ;
#6019 = APPLICATION_PROTOCOL_DEFINITION ( 'draft international standard', 'automotive_design', 1998, #9204 ) ;
#6020 = EDGE_CURVE ( 'NONE', #4808, #5309, #9787, .T. ) ;
#6021 = CIRCLE ( 'NONE', #468, 2.800000000000003819 ) ;
#6022 = AXIS2_PLACEMENT_3D ( 'NONE', #2117, #6035, #6951 ) ;
#6023 = DIRECTION ( 'NONE',  ( 0.000000000000000000, -0.6579387259397028176, -0.7530714660036196273 ) ) ;
#6024 = VERTEX_POINT ( 'NONE', #923 ) ;
#6025 = DIRECTION ( 'NONE',  ( -1.000000000000000000, -1.031065855027150586E-29, 2.218671295934095703E-30 ) ) ;
#6026 = LINE ( 'NONE', #5250, #12418 ) ;
#6027 = VERTEX_POINT ( 'NONE', #4919 ) ;
#6028 = DIRECTION ( 'NONE',  ( 0.000000000000000000, 0.000000000000000000, 1.000000000000000000 ) ) ;
#6029 = CARTESIAN_POINT ( 'NONE',  ( 9.999999999999998224, -3.399584271718289141, -6.572885726945646212 ) ) ;
#6030 = AXIS2_PLACEMENT_3D ( 'NONE', #11305, #9226, #10185 ) ;
#6031 = VERTEX_POINT ( 'NONE', #8780 ) ;
#6032 = ORIENTED_EDGE ( 'NONE', *, *, #3637, .F. ) ;
#6033 = ORIENTED_EDGE ( 'NONE', *, *, #3927, .F. ) ;
#6034 = ORIENTED_EDGE ( 'NONE', *, *, #3986, .F. ) ;
#6035 = DIRECTION ( 'NONE',  ( -0.000000000000000000, -0.000000000000000000, -1.000000000000000000 ) ) ;
#6036 = ADVANCED_FACE ( 'NONE', ( #7874 ), #12724, .F. ) ;
#6037 = CIRCLE ( 'NONE', #10554, 2.800000000000003375 ) ;
#6038 = CARTESIAN_POINT ( 'NONE',  ( -3.472371940585999184, -2.614027278893196193, -3.320322319202239303 ) ) ;
#6039 = ORIENTED_EDGE ( 'NONE', *, *, #6040, .F. ) ;
#6040 = EDGE_CURVE ( 'NONE', #2828, #6343, #957, .T. ) ;
#6041 = CARTESIAN_POINT ( 'NONE',  ( 4.000000000000000000, 0.7924765000094649015, -0.05906175389889841559 ) ) ;
#6042 = ORIENTED_EDGE ( 'NONE', *, *, #2999, .F. ) ;
#6043 = DIRECTION ( 'NONE',  ( 0.000000000000000000, 0.000000000000000000, 1.000000000000000000 ) ) ;
#6044 = ADVANCED_FACE ( 'NONE', ( #2012 ), #5942, .F. ) ;
#6045 = ADVANCED_FACE ( 'NONE', ( #3007 ), #1042, .T. ) ;
#6046 = CARTESIAN_POINT ( 'NONE',  ( 0.000000000000000000, 0.000000000000000000, 0.000000000000000000 ) ) ;
#6047 = CIRCLE ( 'NONE', #2981, 19.99999999999998934 ) ;
#6048 = DIRECTION ( 'NONE',  ( -1.000000000000000000, 1.010728034814421376E-30, 1.090846720500930387E-30 ) ) ;
#6049 = ORIENTED_EDGE ( 'NONE', *, *, #3289, .F. ) ;
#6050 = DIRECTION ( 'NONE',  ( -1.000000000000000000, 0.000000000000000000, 0.000000000000000000 ) ) ;
#6051 = EDGE_LOOP ( 'NONE', ( #5967, #5207, #2377, #10717 ) ) ;
#6052 = CARTESIAN_POINT ( 'NONE',  ( 0.000000000000000000, 7.358375340957004518, -0.7837807994560929137 ) ) ;
#6053 = SURFACE_SIDE_STYLE ('',( #7916 ) ) ;
#6054 = VECTOR ( 'NONE', #1896, 1000.000000000000227 ) ;
#6055 = FACE_OUTER_BOUND ( 'NONE', #9897, .T. ) ;
#6056 = DIRECTION ( 'NONE',  ( 0.000000000000000000, 4.478906847412178337E-32, -1.000000000000000000 ) ) ;
#6057 = EDGE_CURVE ( 'NONE', #4412, #5688, #7537, .T. ) ;
#6058 = CARTESIAN_POINT ( 'NONE',  ( 33.00000000000000000, 30.14235464176399404, -24.26236220746664785 ) ) ;
#6059 = FACE_OUTER_BOUND ( 'NONE', #12004, .T. ) ;
#6060 = AXIS2_PLACEMENT_3D ( 'NONE', #185, #3298, #7972 ) ;
#6061 = CIRCLE ( 'NONE', #9955, 2.800000000000002931 ) ;
#6062 = DIRECTION ( 'NONE',  ( 1.000000000000000000, 5.916456789157575403E-31, -1.577021341797098793E-16 ) ) ;
#6063 = DIRECTION ( 'NONE',  ( -2.280301054154483747E-31, -0.5877852522924802425, 0.8090169943749422332 ) ) ;
#6064 = CARTESIAN_POINT ( 'NONE',  ( 0.000000000000000000, 3.238809497145290539, -5.634457741540130016 ) ) ;
#6065 = EDGE_CURVE ( 'NONE', #7722, #3047, #12297, .T. ) ;
#6066 = VECTOR ( 'NONE', #3609, 1000.000000000000114 ) ;
#6067 = ORIENTED_EDGE ( 'NONE', *, *, #8761, .F. ) ;
#6068 = CIRCLE ( 'NONE', #521, 6.499000000000009436 ) ;
#6069 = DIRECTION ( 'NONE',  ( -1.000000000000000000, 1.010728034814421376E-30, 1.090846720500930387E-30 ) ) ;
#6070 = DIRECTION ( 'NONE',  ( -0.000000000000000000, -1.530455820933490821E-32, 1.000000000000000000 ) ) ;
#6071 = CARTESIAN_POINT ( 'NONE',  ( 19.99999999999999645, 0.000000000000000000, 0.000000000000000000 ) ) ;
#6072 = FACE_OUTER_BOUND ( 'NONE', #7902, .T. ) ;
#6073 = CARTESIAN_POINT ( 'NONE',  ( -18.00000000000001421, -30.00000000000000711, 2.000000000000004885 ) ) ;
#6074 = ORIENTED_EDGE ( 'NONE', *, *, #10121, .F. ) ;
#6075 = FACE_BOUND ( 'NONE', #6886, .T. ) ;
#6076 = CARTESIAN_POINT ( 'NONE',  ( 19.99999999999999645, 6.613766744932249253, 3.319350756342022368 ) ) ;
#6077 = SURFACE_STYLE_USAGE ( .BOTH. , #8065 ) ;
#6078 = AXIS2_PLACEMENT_3D ( 'NONE', #7246, #4210, #341 ) ;
#6079 = ORIENTED_EDGE ( 'NONE', *, *, #11724, .T. ) ;
#6080 = CARTESIAN_POINT ( 'NONE',  ( 0.000000000000000000, 0.000000000000000000, 0.000000000000000000 ) ) ;
#6081 = EDGE_LOOP ( 'NONE', ( #9037, #6201, #2829, #7847 ) ) ;
#6082 = EDGE_LOOP ( 'NONE', ( #947, #2788, #6163, #8928 ) ) ;
#6083 = APPLICATION_PROTOCOL_DEFINITION ( 'draft international standard', 'automotive_design', 1998, #6331 ) ;
#6084 = EDGE_CURVE ( 'NONE', #6170, #5074, #8373, .T. ) ;
#6085 = CARTESIAN_POINT ( 'NONE',  ( 19.99999999999999645, 0.000000000000000000, 0.000000000000000000 ) ) ;
#6086 = ADVANCED_FACE ( 'NONE', ( #8261 ), #11162, .F. ) ;
#6087 = EDGE_LOOP ( 'NONE', ( #4492, #10648 ) ) ;
#6088 = CARTESIAN_POINT ( 'NONE',  ( 19.99999999999999645, 0.000000000000000000, 0.000000000000000000 ) ) ;
#6089 = CARTESIAN_POINT ( 'NONE',  ( 40.00000000000006395, 1.290960574571364216E-15, -20.00000000000000000 ) ) ;
#6090 = ORIENTED_EDGE ( 'NONE', *, *, #9913, .T. ) ;
#6091 =( NAMED_UNIT ( * ) PLANE_ANGLE_UNIT ( ) SI_UNIT ( $, .RADIAN. ) );
#6092 = CARTESIAN_POINT ( 'NONE',  ( 4.000000000000000000, 2.309401076758487381, -4.999999999999984013 ) ) ;
#6093 = AXIS2_PLACEMENT_3D ( 'NONE', #5070, #5197, #232 ) ;
#6094 = DIRECTION ( 'NONE',  ( -1.000000000000000000, 1.010728034814421376E-30, 1.090846720500930387E-30 ) ) ;
#6095 = COLOUR_RGB ( '', 0.72549020, 0.75294118, 0.79215686) ;
#6096 = DIRECTION ( 'NONE',  ( 1.000000000000000000, 1.081682119347366197E-16, -6.938893903907228378E-17 ) ) ;
#6097 = ORIENTED_EDGE ( 'NONE', *, *, #3310, .T. ) ;
#6098 = VERTEX_POINT ( 'NONE', #4206 ) ;
#6099 = ORIENTED_EDGE ( 'NONE', *, *, #4308, .T. ) ;
#6100 = ORIENTED_EDGE ( 'NONE', *, *, #8949, .T. ) ;
#6101 = CIRCLE ( 'NONE', #9181, 7.400000000000009237 ) ;
#6102 = LINE ( 'NONE', #1201, #11999 ) ;
#6103 = CIRCLE ( 'NONE', #10816, 7.400000000000011902 ) ;
#6104 = CARTESIAN_POINT ( 'NONE',  ( -3.540020015735288350, -2.810662092923964739, -3.602146406945708090 ) ) ;
#6105 = ADVANCED_FACE ( 'NONE', ( #7173 ), #818, .F. ) ;
#6106 = ORIENTED_EDGE ( 'NONE', *, *, #11647, .T. ) ;
#6107 = CARTESIAN_POINT ( 'NONE',  ( 0.000000000000000000, -2.171317488608455637, -7.074275960383735296 ) ) ;
#6108 = ORIENTED_EDGE ( 'NONE', *, *, #9762, .F. ) ;
#6109 = CARTESIAN_POINT ( 'NONE',  ( -2.171643655288376884, 3.365003104552322544, -1.490401528079900172E-15 ) ) ;
#6110 = AXIS2_PLACEMENT_3D ( 'NONE', #3675, #1603, #828 ) ;
#6111 = VECTOR ( 'NONE', #2606, 1000.000000000000000 ) ;
#6112 = VECTOR ( 'NONE', #8579, 1000.000000000000000 ) ;
#6113 = CARTESIAN_POINT ( 'NONE',  ( 40.00000000000000000, 39.34792583643766051, -17.06347054209567915 ) ) ;
#6114 = CARTESIAN_POINT ( 'NONE',  ( 9.999999999999994671, 1.764426149628142593, 7.186570834724209433 ) ) ;
#6115 = ORIENTED_EDGE ( 'NONE', *, *, #3844, .T. ) ;
#6116 = DIRECTION ( 'NONE',  ( 0.000000000000000000, 0.000000000000000000, 1.000000000000000000 ) ) ;
#6117 = ORIENTED_EDGE ( 'NONE', *, *, #7544, .F. ) ;
#6118 = CARTESIAN_POINT ( 'NONE',  ( 19.99999999999999645, 0.000000000000000000, 0.000000000000000000 ) ) ;
#6119 = SHAPE_REPRESENTATION_RELATIONSHIP ( 'NONE' , 'NONE' ,  #891, #1117 ) ;
#6120 = ADVANCED_FACE ( 'NONE', ( #3386 ), #10111, .T. ) ;
#6121 = AXIS2_PLACEMENT_3D ( 'NONE', #10004, #8216, #1321 ) ;
#6122 = CARTESIAN_POINT ( 'NONE',  ( -3.999999999999991562, 1.941961291383474952, -0.3515519931180154933 ) ) ;
#6123 = ADVANCED_FACE ( 'NONE', ( #5049 ), #1239, .F. ) ;
#6124 = DIRECTION ( 'NONE',  ( -1.000000000000000000, 1.010728034814421376E-30, 1.090846720500930387E-30 ) ) ;
#6125 = DIRECTION ( 'NONE',  ( -1.000000000000000000, -5.916456789157575403E-31, 1.577021341797098793E-16 ) ) ;
#6126 = EDGE_CURVE ( 'NONE', #3160, #9801, #5908, .T. ) ;
#6127 = DIRECTION ( 'NONE',  ( -1.848892746611746419E-31, -1.000000000000000000, 1.982541115402070533E-16 ) ) ;
#6128 = DIRECTION ( 'NONE',  ( -1.158639454543359162E-30, 0.08963930890342669544, 0.9959742939952396235 ) ) ;
#6129 = DIRECTION ( 'NONE',  ( -1.000000000000000000, 1.010728034814421376E-30, 1.090846720500930387E-30 ) ) ;
#6130 = DIRECTION ( 'NONE',  ( 0.000000000000000000, 0.000000000000000000, 1.000000000000000000 ) ) ;
#6131 =( LENGTH_UNIT ( ) NAMED_UNIT ( * ) SI_UNIT ( .MILLI., .METRE. ) );
#6132 = VERTEX_POINT ( 'NONE', #147 ) ;
#6133 = CARTESIAN_POINT ( 'NONE',  ( -17.00000000000002842, -20.00000000000000000, 12.00000000000003730 ) ) ;
#6134 = DIRECTION ( 'NONE',  ( -1.000000000000000000, -1.081682119347366444E-16, 5.551115123125780237E-17 ) ) ;
#6135 = AXIS2_PLACEMENT_3D ( 'NONE', #4141, #1176, #7046 ) ;
#6136 = CARTESIAN_POINT ( 'NONE',  ( -3.999999999999993339, -0.8382240730042115340, -3.220610619767148020 ) ) ;
#6137 = LINE ( 'NONE', #12072, #2212 ) ;
#6138 = VERTEX_POINT ( 'NONE', #211 ) ;
#6139 = DIRECTION ( 'NONE',  ( 1.159061634649218351E-16, -0.000000000000000000, 1.000000000000000000 ) ) ;
#6140 = DIRECTION ( 'NONE',  ( 0.000000000000000000, -1.000000000000000000, 0.000000000000000000 ) ) ;
#6141 = CARTESIAN_POINT ( 'NONE',  ( 19.99999999999997868, -1.623118704078857499, -6.293050665016890477 ) ) ;
#6142 = ORIENTED_EDGE ( 'NONE', *, *, #10281, .F. ) ;
#6143 = CARTESIAN_POINT ( 'NONE',  ( 19.99999999999999645, 0.000000000000000000, 0.000000000000000000 ) ) ;
#6144 = ORIENTED_EDGE ( 'NONE', *, *, #7752, .T. ) ;
#6145 = MECHANICAL_DESIGN_GEOMETRIC_PRESENTATION_REPRESENTATION (  '', ( #9631 ), #4096 ) ;
#6146 = ORIENTED_EDGE ( 'NONE', *, *, #3967, .F. ) ;
#6147 = CARTESIAN_POINT ( 'NONE',  ( 19.99999999999999645, 5.362412286431453623, 3.809543717993933765 ) ) ;
#6148 = VERTEX_POINT ( 'NONE', #4072 ) ;
#6149 = CYLINDRICAL_SURFACE ( 'NONE', #1494, 2.800000000000003819 ) ;
#6150 = ORIENTED_EDGE ( 'NONE', *, *, #9385, .F. ) ;
#6151 = AXIS2_PLACEMENT_3D ( 'NONE', #8184, #3318, #7233 ) ;
#6152 = DIRECTION ( 'NONE',  ( -1.000000000000000000, 1.010728034814421376E-30, 1.090846720500930387E-30 ) ) ;
#6153 = CARTESIAN_POINT ( 'NONE',  ( 19.99999999999999645, -6.484265599627167198, -1.105616797299011855 ) ) ;
#6154 = FACE_OUTER_BOUND ( 'NONE', #237, .T. ) ;
#6155 = CARTESIAN_POINT ( 'NONE',  ( 20.00000000000000355, 10.26855730552413881, -22.42000078613342851 ) ) ;
#6156 = VECTOR ( 'NONE', #6688, 1000.000000000000000 ) ;
#6157 = ADVANCED_FACE ( 'NONE', ( #11945 ), #1175, .T. ) ;
#6158 = ORIENTED_EDGE ( 'NONE', *, *, #10844, .F. ) ;
#6159 = ORIENTED_EDGE ( 'NONE', *, *, #10099, .F. ) ;
#6160 = ORIENTED_EDGE ( 'NONE', *, *, #7448, .T. ) ;
#6161 = B_SPLINE_CURVE_WITH_KNOTS ( 'NONE', 3,
 ( #2934, #9783, #4782, #5678, #8712, #6783 ),
 .UNSPECIFIED., .F., .F.,
 ( 4, 2, 4 ),
 ( 0.000000000000000000, 0.0002095117440864791795, 0.0004190234881729583589 ),
 .UNSPECIFIED. ) ;
#6162 = CIRCLE ( 'NONE', #2266, 6.499000000000008548 ) ;
#6163 = ORIENTED_EDGE ( 'NONE', *, *, #9263, .F. ) ;
#6164 = VECTOR ( 'NONE', #11416, 1000.000000000000000 ) ;
#6165 = CIRCLE ( 'NONE', #397, 2.800000000000003375 ) ;
#6166 = DIRECTION ( 'NONE',  ( 0.000000000000000000, 0.000000000000000000, 1.000000000000000000 ) ) ;
#6167 = PLANE ( 'NONE',  #5071 ) ;
#6168 = ORIENTED_EDGE ( 'NONE', *, *, #6359, .T. ) ;
#6169 = DIRECTION ( 'NONE',  ( 0.000000000000000000, 0.000000000000000000, -1.000000000000000000 ) ) ;
#6170 = VERTEX_POINT ( 'NONE', #9023 ) ;
#6171 = CARTESIAN_POINT ( 'NONE',  ( 0.000000000000000000, 5.025702764809073742, 5.431603052487396610 ) ) ;
#6172 = AXIS2_PLACEMENT_3D ( 'NONE', #5860, #2861, #10682 ) ;
#6173 = AXIS2_PLACEMENT_3D ( 'NONE', #9380, #8432, #11275 ) ;
#6174 = EDGE_CURVE ( 'NONE', #11698, #8908, #1985, .T. ) ;
#6175 = DIRECTION ( 'NONE',  ( 0.000000000000000000, 0.000000000000000000, 1.000000000000000000 ) ) ;
#6176 = EDGE_CURVE ( 'NONE', #12656, #8701, #5175, .T. ) ;
#6177 = CARTESIAN_POINT ( 'NONE',  ( 19.99999999999997868, 1.764426149628238960, -7.186570834724189005 ) ) ;
#6178 = ORIENTED_EDGE ( 'NONE', *, *, #340, .F. ) ;
#6179 = LINE ( 'NONE', #8599, #10460 ) ;
#6180 = ORIENTED_EDGE ( 'NONE', *, *, #8531, .F. ) ;
#6181 = LINE ( 'NONE', #1345, #7861 ) ;
#6182 = PRESENTATION_LAYER_ASSIGNMENT (  '', '', ( #11741 ) ) ;
#6183 = CIRCLE ( 'NONE', #10676, 6.499000000000010324 ) ;
#6184 = SURFACE_SIDE_STYLE ('',( #2264 ) ) ;
#6185 = CYLINDRICAL_SURFACE ( 'NONE', #11938, 2.000000000000003109 ) ;
#6186 = CARTESIAN_POINT ( 'NONE',  ( 19.99999999999999645, -6.969736844459705871, 2.486517307195113879 ) ) ;
#6187 = ADVANCED_BREP_SHAPE_REPRESENTATION ( '', ( #5724, #12422 ), #3119 ) ;
#6188 = CARTESIAN_POINT ( 'NONE',  ( -0.6666666666666353214, -4.233901974057276973, -3.300726591567087809 ) ) ;
#6189 = DIRECTION ( 'NONE',  ( 0.000000000000000000, 0.000000000000000000, 1.000000000000000000 ) ) ;
#6190 =( GEOMETRIC_REPRESENTATION_CONTEXT ( 3 ) GLOBAL_UNCERTAINTY_ASSIGNED_CONTEXT ( ( #11399 ) ) GLOBAL_UNIT_ASSIGNED_CONTEXT ( ( #255, #4189, #12057 ) ) REPRESENTATION_CONTEXT ( 'NONE', 'WORKASPACE' ) );
#6191 = DIRECTION ( 'NONE',  ( 0.000000000000000000, -0.8805955318567323387, -0.4738686624730094610 ) ) ;
#6192 = CARTESIAN_POINT ( 'NONE',  ( 4.140404888673280048, 2.228338276487438208, -3.686887068327037831 ) ) ;
#6193 = FACE_OUTER_BOUND ( 'NONE', #372, .T. ) ;
#6194 = EDGE_CURVE ( 'NONE', #2754, #10809, #7549, .T. ) ;
#6195 = CIRCLE ( 'NONE', #644, 0.9999999999999974465 ) ;
#6196 = ORIENTED_EDGE ( 'NONE', *, *, #10412, .F. ) ;
#6197 = DIRECTION ( 'NONE',  ( 0.000000000000000000, -0.4338837391175658365, 0.9009688679024154823 ) ) ;
#6198 = DIRECTION ( 'NONE',  ( 2.218671295934093250E-30, -5.551115123125776539E-17, -1.000000000000000000 ) ) ;
#6199 = DIRECTION ( 'NONE',  ( 2.218671295934093250E-30, -5.551115123125776539E-17, -1.000000000000000000 ) ) ;
#6200 = DIRECTION ( 'NONE',  ( -1.000000000000000000, 1.010728034814421376E-30, 1.090846720500930387E-30 ) ) ;
#6201 = ORIENTED_EDGE ( 'NONE', *, *, #10417, .T. ) ;
#6202 = DIRECTION ( 'NONE',  ( 0.000000000000000000, -1.000000000000000000, 0.000000000000000000 ) ) ;
#6203 = CIRCLE ( 'NONE', #8463, 7.400000000000009237 ) ;
#6204 = EDGE_CURVE ( 'NONE', #12214, #6728, #2475, .T. ) ;
#6205 = CARTESIAN_POINT ( 'NONE',  ( -10.00000000000000178, 0.000000000000000000, 0.000000000000000000 ) ) ;
#6206 = EDGE_CURVE ( 'NONE', #7420, #4162, #6594, .T. ) ;
#6207 = VECTOR ( 'NONE', #6974, 1000.000000000000114 ) ;
#6208 = ORIENTED_EDGE ( 'NONE', *, *, #4099, .T. ) ;
#6209 = DIRECTION ( 'NONE',  ( 0.000000000000000000, 0.000000000000000000, 1.000000000000000000 ) ) ;
#6210 = VERTEX_POINT ( 'NONE', #4463 ) ;
#6211 = VERTEX_POINT ( 'NONE', #591 ) ;
#6212 = CONTEXT_DEPENDENT_SHAPE_REPRESENTATION ( #9606, #11823 ) ;
#6213 = ORIENTED_EDGE ( 'NONE', *, *, #8187, .T. ) ;
#6214 = CARTESIAN_POINT ( 'NONE',  ( 19.99999999999999645, 0.000000000000000000, 0.000000000000000000 ) ) ;
#6215 = VECTOR ( 'NONE', #2263, 1000.000000000000000 ) ;
#6216 = CARTESIAN_POINT ( 'NONE',  ( 0.000000000000000000, 0.000000000000000000, 0.000000000000000000 ) ) ;
#6217 = CYLINDRICAL_SURFACE ( 'NONE', #6373, 3.500000000000003997 ) ;
#6218 = CARTESIAN_POINT ( 'NONE',  ( 19.99999999999999645, 2.180689217871860652, 6.122221454264574092 ) ) ;
#6219 = CARTESIAN_POINT ( 'NONE',  ( 20.00000000000000000, 11.34118543499637077, -24.03007857557328464 ) ) ;
#6220 = EDGE_CURVE ( 'NONE', #11818, #3532, #12396, .T. ) ;
#6221 = CARTESIAN_POINT ( 'NONE',  ( 14.00000000000000000, 61.31370849898475228, 0.000000000000000000 ) ) ;
#6222 = VERTEX_POINT ( 'NONE', #4531 ) ;
#6223 = ORIENTED_EDGE ( 'NONE', *, *, #9415, .T. ) ;
#6224 = AXIS2_PLACEMENT_3D ( 'NONE', #2346, #10170, #1362 ) ;
#6225 = EDGE_CURVE ( 'NONE', #8279, #1374, #9183, .T. ) ;
#6226 = ORIENTED_EDGE ( 'NONE', *, *, #296, .F. ) ;
#6227 = CIRCLE ( 'NONE', #873, 4.000000000000008882 ) ;
#6228 = ORIENTED_EDGE ( 'NONE', *, *, #4598, .T. ) ;
#6229 = DIRECTION ( 'NONE',  ( -1.000000000000000000, 0.000000000000000000, 0.000000000000000000 ) ) ;
#6230 = ADVANCED_FACE ( 'NONE', ( #1689 ), #11289, .T. ) ;
#6231 = CARTESIAN_POINT ( 'NONE',  ( -2.742827927723363590, -3.035229711104975081, -3.433252694550608553 ) ) ;
#6232 = ORIENTED_EDGE ( 'NONE', *, *, #4523, .T. ) ;
#6233 = FACE_OUTER_BOUND ( 'NONE', #6888, .T. ) ;
#6234 = VERTEX_POINT ( 'NONE', #7615 ) ;
#6235 = CIRCLE ( 'NONE', #6660, 4.000000000000000000 ) ;
#6236 = DIRECTION ( 'NONE',  ( 0.000000000000000000, 5.551115123125776539E-17, 1.000000000000000000 ) ) ;
#6237 = CARTESIAN_POINT ( 'NONE',  ( 19.99999999999999645, 0.000000000000000000, 0.000000000000000000 ) ) ;
#6238 = CARTESIAN_POINT ( 'NONE',  ( 3.522875095019549985, -2.820352903225599395, -3.598441714920586953 ) ) ;
#6239 = EDGE_CURVE ( 'NONE', #8666, #8458, #10305, .T. ) ;
#6240 = DIRECTION ( 'NONE',  ( -1.000000000000000000, 0.000000000000000000, 0.000000000000000000 ) ) ;
#6241 = ORIENTED_EDGE ( 'NONE', *, *, #772, .T. ) ;
#6242 = AXIS2_PLACEMENT_3D ( 'NONE', #5048, #10895, #5941 ) ;
#6243 = ORIENTED_EDGE ( 'NONE', *, *, #1839, .F. ) ;
#6244 = FACE_OUTER_BOUND ( 'NONE', #9443, .T. ) ;
#6245 = EDGE_CURVE ( 'NONE', #6872, #574, #6463, .T. ) ;
#6246 = CARTESIAN_POINT ( 'NONE',  ( 2.000000000000001776, 0.000000000000000000, 0.000000000000000000 ) ) ;
#6247 = EDGE_CURVE ( 'NONE', #3660, #11576, #7761, .T. ) ;
#6248 = FACE_OUTER_BOUND ( 'NONE', #1862, .T. ) ;
#6249 = ADVANCED_FACE ( 'NONE', ( #5426 ), #8449, .T. ) ;
#6250 = VECTOR ( 'NONE', #12395, 1000.000000000000000 ) ;
#6251 = CARTESIAN_POINT ( 'NONE',  ( 4.211399257449711442, -2.459727064652543316, -3.751161691472425730 ) ) ;
#6252 = DIRECTION ( 'NONE',  ( -0.000000000000000000, -1.000000000000000000, 0.000000000000000000 ) ) ;
#6253 = CARTESIAN_POINT ( 'NONE',  ( 19.99999999999997868, 6.496448636052932990, -0.1820882179769736653 ) ) ;
#6254 = ORIENTED_EDGE ( 'NONE', *, *, #3842, .F. ) ;
#6255 = DIRECTION ( 'NONE',  ( 0.000000000000000000, -0.7818314824680222541, -0.6234898018587429203 ) ) ;
#6256 = CIRCLE ( 'NONE', #288, 2.149999999999985256 ) ;
#6257 = CARTESIAN_POINT ( 'NONE',  ( 9.285714285714284699, 13.00000000000000000, -3.711537444790451001 ) ) ;
#6258 = EDGE_CURVE ( 'NONE', #1077, #12174, #8387, .T. ) ;
#6259 = VERTEX_POINT ( 'NONE', #9340 ) ;
#6260 = DIRECTION ( 'NONE',  ( 0.000000000000000000, 0.000000000000000000, -1.000000000000000000 ) ) ;
#6261 = DIRECTION ( 'NONE',  ( -1.000000000000000000, 1.010728034814421376E-30, 1.090846720500930387E-30 ) ) ;
#6262 = CARTESIAN_POINT ( 'NONE',  ( -4.197312064133464915, -0.8182229787990212833, -3.502518405183899564 ) ) ;
#6263 = CARTESIAN_POINT ( 'NONE',  ( 4.211140560182228043, -2.431303136016558231, -3.745885042887437510 ) ) ;
#6264 = VECTOR ( 'NONE', #10604, 1000.000000000000000 ) ;
#6265 = CARTESIAN_POINT ( 'NONE',  ( 40.00000000000000711, 14.50364731389636574, -24.59751492040896892 ) ) ;
#6266 = DIRECTION ( 'NONE',  ( 1.000000000000000000, 1.849040895279789448E-31, -6.938893903907224680E-17 ) ) ;
#6267 = EDGE_CURVE ( 'NONE', #10402, #7997, #2743, .T. ) ;
#6268 = PRODUCT_DEFINITION_SHAPE ( 'NONE', 'NONE',  #5937 ) ;
#6269 = ADVANCED_FACE ( 'NONE', ( #5558 ), #8510, .T. ) ;
#6270 = EDGE_LOOP ( 'NONE', ( #3600, #12413, #9238, #2956 ) ) ;
#6271 = CARTESIAN_POINT ( 'NONE',  ( -4.024497503033714452, 2.323544716729490478, -3.572167766733773675 ) ) ;
#6272 = ORIENTED_EDGE ( 'NONE', *, *, #3145, .F. ) ;
#6273 = VECTOR ( 'NONE', #4896, 1000.000000000000000 ) ;
#6274 = EDGE_LOOP ( 'NONE', ( #9487, #12026, #8897, #6090, #8034, #9664, #3518, #5812, #10137, #8011, #3303, #12052, #600, #4485, #11271, #7642, #7075, #7947, #11319, #887, #8097, #9927, #1185, #8156, #4054, #11449, #5624, #2179, #3033, #1633, #4375, #10623, #4979, #7639, #3418, #6496, #2891, #10329, #7559, #4302, #3725, #5769, #10745, #11851, #4248, #7013, #69, #667, #5512, #12465, #11631, #1518, #10257, #7661, #2108, #8071, #11472, #8471, #11109, #8910, #8912, #1070, #2903, #5761, #3077, #11651, #8031, #3383, #8789, #806, #4620, #5315, #510, #3037, #647, #5886, #7213, #1197, #8318, #4035, #12447, #3863, #6362, #9053, #4294, #5371, #7587, #3476, #3732, #3657, #3126, #1061, #5065, #2501, #7054, #5268, #10707, #1729, #3287, #5896, #6039, #10092, #10893, #11012, #3003, #10286, #10419, #1485, #5964, #1975, #7294, #9511, #7651, #3805, #10663, #11962, #11628, #10713, #12473, #7508, #8350, #6824, #8989, #12377, #9813, #9561, #12613, #4800, #678, #4102, #2409, #9757, #116, #5458, #3990, #6213, #11188, #3954, #2094, #2552, #6478, #10972, #150, #11499 ) ) ;
#6275 = CONTEXT_DEPENDENT_SHAPE_REPRESENTATION ( #7658, #7592 ) ;
#6276 = AXIS2_PLACEMENT_3D ( 'NONE', #5381, #4354, #12289 ) ;
#6277 = VERTEX_POINT ( 'NONE', #5616 ) ;
#6278 = EDGE_CURVE ( 'NONE', #5156, #10905, #10798, .T. ) ;
#6279 = CARTESIAN_POINT ( 'NONE',  ( -4.000000000000012434, 2.309401076758501592, -3.433295621305395340 ) ) ;
#6280 = EDGE_CURVE ( 'NONE', #11478, #8279, #3448, .T. ) ;
#6281 = SURFACE_STYLE_USAGE ( .BOTH. , #8339 ) ;
#6282 = DIRECTION ( 'NONE',  ( -3.437775699846489820E-17, -0.2951046417778627751, -0.9554649393887560960 ) ) ;
#6283 = CARTESIAN_POINT ( 'NONE',  ( 19.99999999999999645, -0.8732627748488548391, 7.348293143721422283 ) ) ;
#6284 = ORIENTED_EDGE ( 'NONE', *, *, #9876, .T. ) ;
#6285 = CARTESIAN_POINT ( 'NONE',  ( -4.141042297810622053, 2.227970268150405886, -3.687027686973636253 ) ) ;
#6286 = AXIS2_PLACEMENT_3D ( 'NONE', #4845, #10694, #5744 ) ;
#6287 = EDGE_CURVE ( 'NONE', #87, #2228, #5282, .T. ) ;
#6288 = FACE_OUTER_BOUND ( 'NONE', #1867, .T. ) ;
#6289 = ORIENTED_EDGE ( 'NONE', *, *, #12183, .F. ) ;
#6290 = ORIENTED_EDGE ( 'NONE', *, *, #715, .T. ) ;
#6291 = VERTEX_POINT ( 'NONE', #3818 ) ;
#6292 = VERTEX_POINT ( 'NONE', #10631 ) ;
#6293 = CARTESIAN_POINT ( 'NONE',  ( 0.000000000000000000, 1.531833341630128409, 6.396997380212699369 ) ) ;
#6294 = SURFACE_STYLE_USAGE ( .BOTH. , #6356 ) ;
#6295 = ORIENTED_EDGE ( 'NONE', *, *, #5262, .F. ) ;
#6296 = CIRCLE ( 'NONE', #3029, 6.499000000000009436 ) ;
#6297 = CARTESIAN_POINT ( 'NONE',  ( -10.00000000000000178, 0.000000000000000000, 0.000000000000000000 ) ) ;
#6298 = ORIENTED_EDGE ( 'NONE', *, *, #754, .T. ) ;
#6299 = CARTESIAN_POINT ( 'NONE',  ( -3.861362476283222378, -2.629030857716012637, -3.671615880910391372 ) ) ;
#6300 = CARTESIAN_POINT ( 'NONE',  ( 0.000000000000000000, 0.000000000000000000, 0.000000000000000000 ) ) ;
#6301 = DIRECTION ( 'NONE',  ( 0.000000000000000000, 0.000000000000000000, 1.000000000000000000 ) ) ;
#6302 = AXIS2_PLACEMENT_3D ( 'NONE', #10585, #861, #3953 ) ;
#6303 = CARTESIAN_POINT ( 'NONE',  ( 6.000000000000000000, 49.63999999999998636, -13.00000000000000178 ) ) ;
#6304 = AXIS2_PLACEMENT_3D ( 'NONE', #6216, #356, #483 ) ;
#6305 = ORIENTED_EDGE ( 'NONE', *, *, #9473, .T. ) ;
#6306 = VERTEX_POINT ( 'NONE', #11865 ) ;
#6307 = LINE ( 'NONE', #8243, #7040 ) ;
#6308 = CARTESIAN_POINT ( 'NONE',  ( 0.000000000000000000, 0.000000000000000000, 0.000000000000000000 ) ) ;
#6309 = LINE ( 'NONE', #12120, #5152 ) ;
#6310 = AXIS2_PLACEMENT_3D ( 'NONE', #9632, #10422, #5720 ) ;
#6311 = AXIS2_PLACEMENT_3D ( 'NONE', #6720, #12588, #11556 ) ;
#6312 = CARTESIAN_POINT ( 'NONE',  ( 0.000000000000000000, 0.000000000000000000, 0.000000000000000000 ) ) ;
#6313 = AXIS2_PLACEMENT_3D ( 'NONE', #7681, #12710, #1935 ) ;
#6314 = LINE ( 'NONE', #1348, #3436 ) ;
#6315 = DIRECTION ( 'NONE',  ( -1.000000000000000000, -1.081682119347366197E-16, 6.938893903907228378E-17 ) ) ;
#6316 = DIRECTION ( 'NONE',  ( -1.000000000000000000, -5.916456789157575403E-31, 1.224646799147352714E-16 ) ) ;
#6317 = EDGE_CURVE ( 'NONE', #10794, #2160, #8575, .T. ) ;
#6318 = VERTEX_POINT ( 'NONE', #4905 ) ;
#6319 = CYLINDRICAL_SURFACE ( 'NONE', #8640, 2.000000000000000888 ) ;
#6320 = EDGE_CURVE ( 'NONE', #125, #6740, #2634, .T. ) ;
#6321 = DIRECTION ( 'NONE',  ( 0.000000000000000000, 0.000000000000000000, -1.000000000000000000 ) ) ;
#6322 = VERTEX_POINT ( 'NONE', #9782 ) ;
#6323 = DIRECTION ( 'NONE',  ( 1.000000000000000000, -1.010728034814421376E-30, -1.090846720500930387E-30 ) ) ;
#6324 = DIRECTION ( 'NONE',  ( 0.000000000000000000, 0.9510565162951544194, -0.3090169943749445092 ) ) ;
#6325 = DIRECTION ( 'NONE',  ( -1.000000000000000000, 1.010728034814421376E-30, 1.090846720500930387E-30 ) ) ;
#6326 = CARTESIAN_POINT ( 'NONE',  ( 4.000000000000022204, -2.309401076758519800, -3.504271511727111044 ) ) ;
#6327 = CARTESIAN_POINT ( 'NONE',  ( 19.99999999999999645, 0.000000000000000000, 0.000000000000000000 ) ) ;
#6328 = CARTESIAN_POINT ( 'NONE',  ( 19.99999999999999645, 0.000000000000000000, 0.000000000000000000 ) ) ;
#6329 = EDGE_CURVE ( 'NONE', #8944, #2437, #11738, .T. ) ;
#6330 = CARTESIAN_POINT ( 'NONE',  ( 0.000000000000000000, -0.8865213383406727043, 1.535500000000009191 ) ) ;
#6331 = APPLICATION_CONTEXT ( 'automotive_design' ) ;
#6332 = ORIENTED_EDGE ( 'NONE', *, *, #4360, .F. ) ;
#6333 = CARTESIAN_POINT ( 'NONE',  ( -4.000000000000015099, 2.309401076758498927, -3.504269196027880895 ) ) ;
#6334 = ORIENTED_EDGE ( 'NONE', *, *, #1157, .F. ) ;
#6335 = ORIENTED_EDGE ( 'NONE', *, *, #3547, .T. ) ;
#6336 = ITEM_DEFINED_TRANSFORMATION ( 'NONE', 'NONE', #8369,  #12422 ) ;
#6337 = CIRCLE ( 'NONE', #1015, 7.400000000000011902 ) ;
#6338 = ORIENTED_EDGE ( 'NONE', *, *, #10201, .F. ) ;
#6339 = CARTESIAN_POINT ( 'NONE',  ( -35.00000000000006395, -30.00000000000000000, 2.218822049206081369E-15 ) ) ;
#6340 = FACE_OUTER_BOUND ( 'NONE', #11330, .T. ) ;
#6341 = DIRECTION ( 'NONE',  ( -0.9396926207859086499, -1.281224895503606024E-31, -0.3420201433256680468 ) ) ;
#6342 = CYLINDRICAL_SURFACE ( 'NONE', #1978, 2.149999999999999023 ) ;
#6343 = VERTEX_POINT ( 'NONE', #9715 ) ;
#6344 = DIRECTION ( 'NONE',  ( 1.000000000000000000, -1.010728034814421376E-30, -1.090846720500930387E-30 ) ) ;
#6345 = EDGE_CURVE ( 'NONE', #4493, #2734, #10626, .T. ) ;
#6346 = AXIS2_PLACEMENT_3D ( 'NONE', #3538, #6558, #7712 ) ;
#6347 = CARTESIAN_POINT ( 'NONE',  ( 19.99999999999999645, -0.8135880386783197471, 6.527339685683405612 ) ) ;
#6348 = EDGE_LOOP ( 'NONE', ( #12360, #1601, #5136, #9462 ) ) ;
#6349 = EDGE_CURVE ( 'NONE', #4250, #11665, #2868, .T. ) ;
#6350 = ORIENTED_EDGE ( 'NONE', *, *, #4980, .F. ) ;
#6351 = ORIENTED_EDGE ( 'NONE', *, *, #12089, .T. ) ;
#6352 = ADVANCED_FACE ( 'NONE', ( #5742 ), #6908, .T. ) ;
#6353 = ORIENTED_EDGE ( 'NONE', *, *, #3364, .F. ) ;
#6354 = FACE_OUTER_BOUND ( 'NONE', #2309, .T. ) ;
#6355 = CIRCLE ( 'NONE', #6151, 4.000000000000000000 ) ;
#6357 = CONICAL_SURFACE ( 'NONE', #2256, 1.610000000000001874, 0.7853981633974658205 ) ;
#6356 = SURFACE_SIDE_STYLE ('',( #2571 ) ) ;
#6358 = EDGE_LOOP ( 'NONE', ( #3846, #2214, #5199, #5158 ) ) ;
#6359 = EDGE_CURVE ( 'NONE', #640, #1141, #6782, .T. ) ;
#6360 = LINE ( 'NONE', #567, #9628 ) ;
#6361 = CONICAL_SURFACE ( 'NONE', #9221, 5.560781378645573980, 1.221730476396046816 ) ;
#6362 = ORIENTED_EDGE ( 'NONE', *, *, #11241, .T. ) ;
#6363 = DIRECTION ( 'NONE',  ( -1.000000000000000000, 1.010728034814421376E-30, 1.090846720500930387E-30 ) ) ;
#6364 = CARTESIAN_POINT ( 'NONE',  ( 12.94787914004603557, 12.50000000000000000, 5.638155724715463890 ) ) ;
#6365 = DIRECTION ( 'NONE',  ( -1.000000000000000000, 1.010728034814421376E-30, 1.090846720500930387E-30 ) ) ;
#6366 = AXIS2_PLACEMENT_3D ( 'NONE', #10620, #11727, #2924 ) ;
#6367 = STYLED_ITEM ( 'NONE', ( #11365 ), #10172 ) ;
#6368 = CIRCLE ( 'NONE', #8002, 2.500000000000003553 ) ;
#6369 = EDGE_CURVE ( 'NONE', #1582, #10108, #9655, .T. ) ;
#6370 = DIRECTION ( 'NONE',  ( -1.000000000000000000, 1.010728034814421376E-30, 1.090846720500930387E-30 ) ) ;
#6371 = EDGE_CURVE ( 'NONE', #561, #9770, #971, .T. ) ;
#6372 = ORIENTED_EDGE ( 'NONE', *, *, #6369, .F. ) ;
#6373 = AXIS2_PLACEMENT_3D ( 'NONE', #2304, #5131, #7322 ) ;
#6374 = ORIENTED_EDGE ( 'NONE', *, *, #7586, .F. ) ;
#6375 = DIRECTION ( 'NONE',  ( -4.930380657631325535E-31, -1.000000000000000000, -1.177425296209239362E-30 ) ) ;
#6376 = CYLINDRICAL_SURFACE ( 'NONE', #5756, 2.800000000000003819 ) ;
#6377 = VECTOR ( 'NONE', #2325, 1000.000000000000000 ) ;
#6378 = VECTOR ( 'NONE', #6519, 1000.000000000000000 ) ;
#6379 = VECTOR ( 'NONE', #577, 1000.000000000000000 ) ;
#6380 = DIRECTION ( 'NONE',  ( 0.000000000000000000, 6.839766848137126197E-14, -1.000000000000000000 ) ) ;
#6381 = FACE_OUTER_BOUND ( 'NONE', #166, .T. ) ;
#6382 = DIRECTION ( 'NONE',  ( 1.000000000000000000, -1.010728034814421376E-30, -1.090846720500930387E-30 ) ) ;
#6383 = CARTESIAN_POINT ( 'NONE',  ( 19.99999999999999645, -6.577476285968334224, -0.06996125000500313940 ) ) ;
#6384 = ORIENTED_EDGE ( 'NONE', *, *, #11480, .T. ) ;
#6385 = CARTESIAN_POINT ( 'NONE',  ( 2.742827927723509696, 3.035229711105237538, -3.433252694550597450 ) ) ;
#6386 = AXIS2_PLACEMENT_3D ( 'NONE', #10347, #9375, #9315 ) ;
#6387 = AXIS2_PLACEMENT_3D ( 'NONE', #6297, #9187, #8232 ) ;
#6388 = CYLINDRICAL_SURFACE ( 'NONE', #7853, 2.800000000000003819 ) ;
#6389 = ADVANCED_FACE ( 'NONE', ( #14 ), #1032, .T. ) ;
#6390 =( NAMED_UNIT ( * ) PLANE_ANGLE_UNIT ( ) SI_UNIT ( $, .RADIAN. ) );
#6391 = EDGE_CURVE ( 'NONE', #8587, #4499, #2933, .T. ) ;
#6392 = DIRECTION ( 'NONE',  ( -1.000000000000000000, 1.010728034814421376E-30, 1.090846720500930387E-30 ) ) ;
#6393 = ORIENTED_EDGE ( 'NONE', *, *, #8248, .T. ) ;
#6394 = CARTESIAN_POINT ( 'NONE',  ( 40.00000000000000711, 40.41548023366552655, -10.14535464186970692 ) ) ;
#6395 = FACE_OUTER_BOUND ( 'NONE', #96, .T. ) ;
#6396 =( GEOMETRIC_REPRESENTATION_CONTEXT ( 3 ) GLOBAL_UNCERTAINTY_ASSIGNED_CONTEXT ( ( #6634 ) ) GLOBAL_UNIT_ASSIGNED_CONTEXT ( ( #10560, #8639, #11483 ) ) REPRESENTATION_CONTEXT ( 'NONE', 'WORKASPACE' ) );
#6397 = DIRECTION ( 'NONE',  ( -1.000000000000000000, 1.006188713385347367E-17, 3.844790828812615713E-17 ) ) ;
#6398 = CARTESIAN_POINT ( 'NONE',  ( -9.000000000000000000, 49.63999999999998636, -13.00000000000000178 ) ) ;
#6399 = CARTESIAN_POINT ( 'NONE',  ( 14.00000000000000000, 30.00000000000000000, 0.000000000000000000 ) ) ;
#6400 = DIRECTION ( 'NONE',  ( 1.380506584136768733E-30, -0.5128992774058949156, -0.8584487936018728726 ) ) ;
#6401 = CARTESIAN_POINT ( 'NONE',  ( 9.000000000000035527, 30.00000000000000000, 25.00000000000007105 ) ) ;
#6402 = ORIENTED_EDGE ( 'NONE', *, *, #6586, .F. ) ;
#6403 = CARTESIAN_POINT ( 'NONE',  ( -4.000000000000012434, 2.309401076758501592, -3.433295621305395340 ) ) ;
#6404 = ORIENTED_EDGE ( 'NONE', *, *, #12091, .F. ) ;
#6405 = VECTOR ( 'NONE', #10312, 1000.000000000000000 ) ;
#6406 = CONTEXT_DEPENDENT_SHAPE_REPRESENTATION ( #8555, #9556 ) ;
#6407 = B_SPLINE_CURVE_WITH_KNOTS ( 'NONE', 3,
 ( #1950, #4667, #9665, #12660, #1700 ),
 .UNSPECIFIED., .F., .F.,
 ( 4, 1, 4 ),
 ( 0.000000000000000000, 0.002309401076758506224, 0.004618802153517012447 ),
 .UNSPECIFIED. ) ;
#6408 = ORIENTED_EDGE ( 'NONE', *, *, #323, .T. ) ;
#6409 = ORIENTED_EDGE ( 'NONE', *, *, #11138, .T. ) ;
#6410 = EDGE_CURVE ( 'NONE', #5127, #1397, #759, .T. ) ;
#6411 = DIRECTION ( 'NONE',  ( -1.000000000000000000, 1.010728034814421376E-30, 1.090846720500930387E-30 ) ) ;
#6412 = EDGE_CURVE ( 'NONE', #11656, #4395, #10427, .T. ) ;
#6413 = LINE ( 'NONE', #12662, #6525 ) ;
#6415 = ADVANCED_FACE ( 'NONE', ( #1878 ), #9841, .T. ) ;
#6414 = DIRECTION ( 'NONE',  ( -1.000000000000000000, 1.010728034814421376E-30, 1.090846720500930387E-30 ) ) ;
#6416 = AXIS2_PLACEMENT_3D ( 'NONE', #3556, #9450, #2528 ) ;
#6417 = CARTESIAN_POINT ( 'NONE',  ( 19.99999999999999645, -6.133480037816503305, 2.376659734729468010 ) ) ;
#6418 = ORIENTED_EDGE ( 'NONE', *, *, #9688, .T. ) ;
#6419 = EDGE_CURVE ( 'NONE', #5144, #4279, #4972, .T. ) ;
#6420 = PLANE ( 'NONE',  #10375 ) ;
#6421 = VECTOR ( 'NONE', #1421, 1000.000000000000000 ) ;
#6422 = LINE ( 'NONE', #3344, #4113 ) ;
#6423 = ORIENTED_EDGE ( 'NONE', *, *, #1370, .T. ) ;
#6424 = EDGE_LOOP ( 'NONE', ( #8153, #3961, #12502, #10488 ) ) ;
#6425 = CARTESIAN_POINT ( 'NONE',  ( -9.000000000000000000, 49.63999999999998636, -13.00000000000000178 ) ) ;
#6426 = ORIENTED_EDGE ( 'NONE', *, *, #9595, .T. ) ;
#6427 = ORIENTED_EDGE ( 'NONE', *, *, #8803, .F. ) ;
#6428 = DIRECTION ( 'NONE',  ( 1.000000000000000000, 0.000000000000000000, 0.000000000000000000 ) ) ;
#6429 = CIRCLE ( 'NONE', #659, 7.400000000000011902 ) ;
#6430 = DIRECTION ( 'NONE',  ( 1.577021341797099039E-16, 1.177425296209237084E-30, 1.000000000000000000 ) ) ;
#6431 = ORIENTED_EDGE ( 'NONE', *, *, #715, .F. ) ;
#6432 = CARTESIAN_POINT ( 'NONE',  ( 19.99999999999997868, 4.596015818000145359, -4.705818469689468486 ) ) ;
#6433 = DIRECTION ( 'NONE',  ( 0.000000000000000000, -0.2660368455666825005, 0.9639628606958513535 ) ) ;
#6434 = EDGE_LOOP ( 'NONE', ( #5387, #4868, #9134, #4171 ) ) ;
#6435 = EDGE_CURVE ( 'NONE', #2491, #11340, #3453, .T. ) ;
#6436 = CARTESIAN_POINT ( 'NONE',  ( 19.99999999999997868, -3.426907987218776874, -5.522074125465566752 ) ) ;
#6437 = CARTESIAN_POINT ( 'NONE',  ( 19.99999999999999645, 0.000000000000000000, 0.000000000000000000 ) ) ;
#6438 = AXIS2_PLACEMENT_3D ( 'NONE', #7043, #9916, #336 ) ;
#6439 = LINE ( 'NONE', #8483, #311 ) ;
#6440 = CIRCLE ( 'NONE', #11166, 2.800000000000002931 ) ;
#6441 = DIRECTION ( 'NONE',  ( 0.000000000000000000, 0.000000000000000000, 1.000000000000000000 ) ) ;
#6442 = ADVANCED_FACE ( 'NONE', ( #3876 ), #7921, .T. ) ;
#6443 = ORIENTED_EDGE ( 'NONE', *, *, #1398, .F. ) ;
#6444 = ORIENTED_EDGE ( 'NONE', *, *, #6834, .F. ) ;
#6445 = PLANE ( 'NONE',  #7666 ) ;
#6446 = AXIS2_PLACEMENT_3D ( 'NONE', #4971, #9713, #9780 ) ;
#6447 = CARTESIAN_POINT ( 'NONE',  ( 19.99999999999999645, -6.577476285968334224, -0.06996125000500313940 ) ) ;
#6448 = VECTOR ( 'NONE', #1266, 1000.000000000000000 ) ;
#6449 = EDGE_CURVE ( 'NONE', #3887, #2848, #8107, .T. ) ;
#6450 = CARTESIAN_POINT ( 'NONE',  ( 33.00000000000001421, 39.34792583643766761, -17.06347054209568270 ) ) ;
#6451 = LINE ( 'NONE', #10359, #8557 ) ;
#6452 = CYLINDRICAL_SURFACE ( 'NONE', #299, 6.499000000000010324 ) ;
#6453 = AXIS2_PLACEMENT_3D ( 'NONE', #9153, #11814, #3006 ) ;
#6454 = DIRECTION ( 'NONE',  ( 0.000000000000000000, 0.000000000000000000, 1.000000000000000000 ) ) ;
#6455 = EDGE_LOOP ( 'NONE', ( #3353, #12393, #11072, #4405, #7881, #9758, #10702, #428, #12101 ) ) ;
#6456 = CARTESIAN_POINT ( 'NONE',  ( 0.000000000000000000, 0.000000000000000000, 0.000000000000000000 ) ) ;
#6457 = CARTESIAN_POINT ( 'NONE',  ( 14.00000000000000000, -30.00000000000000000, -4.000000000000000000 ) ) ;
#6458 = CARTESIAN_POINT ( 'NONE',  ( 4.000000000000002665, 1.539600717838986110, -3.300726591567064716 ) ) ;
#6459 = VECTOR ( 'NONE', #1688, 1000.000000000000000 ) ;
#6460 = VERTEX_POINT ( 'NONE', #6968 ) ;
#6461 = CARTESIAN_POINT ( 'NONE',  ( 19.99999999999999645, 0.000000000000000000, 0.000000000000000000 ) ) ;
#6462 = DIRECTION ( 'NONE',  ( -1.000000000000000000, 1.010728034814421376E-30, 1.090846720500930387E-30 ) ) ;
#6463 = LINE ( 'NONE', #9279, #563 ) ;
#6464 = FACE_OUTER_BOUND ( 'NONE', #3333, .T. ) ;
#6465 = CARTESIAN_POINT ( 'NONE',  ( 9.999999999999994671, -7.258495115966563382, -1.440225208600910634 ) ) ;
#6466 = B_SPLINE_CURVE_WITH_KNOTS ( 'NONE', 3,
 ( #182, #373, #4112, #3357, #7276, #11199, #6299, #10208 ),
 .UNSPECIFIED., .F., .F.,
 ( 4, 2, 2, 4 ),
 ( 0.000000000000000000, 0.002450665683189819262, 0.003675998524784728893, 0.004901331366379638524 ),
 .UNSPECIFIED. ) ;
#6467 = CIRCLE ( 'NONE', #8926, 6.499000000000011212 ) ;
#6468 = CARTESIAN_POINT ( 'NONE',  ( 9.999999999999994671, -3.399584271718382844, 6.572885726945587592 ) ) ;
#6469 = EDGE_CURVE ( 'NONE', #12527, #8854, #12302, .T. ) ;
#6470 = DIRECTION ( 'NONE',  ( -1.000000000000000000, 0.000000000000000000, 0.000000000000000000 ) ) ;
#6471 = AXIS2_PLACEMENT_3D ( 'NONE', #8859, #4812, #8676 ) ;
#6472 = CARTESIAN_POINT ( 'NONE',  ( 0.000000000000000000, 0.000000000000000000, 0.000000000000000000 ) ) ;
#6473 = ORIENTED_EDGE ( 'NONE', *, *, #8108, .T. ) ;
#6474 = CONTEXT_DEPENDENT_SHAPE_REPRESENTATION ( #10938, #3999 ) ;
#6475 = CIRCLE ( 'NONE', #1335, 7.400000000000009237 ) ;
#6476 = ORIENTED_EDGE ( 'NONE', *, *, #112, .T. ) ;
#6477 = AXIS2_PLACEMENT_3D ( 'NONE', #12557, #3730, #4758 ) ;
#6478 = ORIENTED_EDGE ( 'NONE', *, *, #12679, .T. ) ;
#6479 = CARTESIAN_POINT ( 'NONE',  ( 0.000000000000000000, 0.000000000000000000, 0.000000000000000000 ) ) ;
#6480 = DIRECTION ( 'NONE',  ( 0.000000000000000000, 0.8805955318567392220, -0.4738686624729965269 ) ) ;
#6481 = DIRECTION ( 'NONE',  ( 1.140150527077241873E-30, 0.000000000000000000, -1.000000000000000000 ) ) ;
#6482 = CARTESIAN_POINT ( 'NONE',  ( 0.000000000000000000, -5.492355906873351401, -4.959236492872013180 ) ) ;
#6483 = ORIENTED_EDGE ( 'NONE', *, *, #7692, .F. ) ;
#6484 = CARTESIAN_POINT ( 'NONE',  ( 9.000000000000031974, 12.50000000000000000, -1.576761677324514786E-16 ) ) ;
#6485 = DIRECTION ( 'NONE',  ( 0.000000000000000000, 0.000000000000000000, 1.000000000000000000 ) ) ;
#6486 = ORIENTED_EDGE ( 'NONE', *, *, #9838, .F. ) ;
#6487 = CIRCLE ( 'NONE', #918, 2.800000000000004263 ) ;
#6488 = AXIS2_PLACEMENT_3D ( 'NONE', #3894, #9796, #11689 ) ;
#6489 = ORIENTED_EDGE ( 'NONE', *, *, #450, .F. ) ;
#6490 = EDGE_CURVE ( 'NONE', #1849, #479, #7339, .T. ) ;
#6491 = FACE_BOUND ( 'NONE', #4928, .T. ) ;
#6492 = ORIENTED_EDGE ( 'NONE', *, *, #9231, .T. ) ;
#6493 = ADVANCED_FACE ( 'NONE', ( #9191 ), #7980, .T. ) ;
#6494 = ORIENTED_EDGE ( 'NONE', *, *, #4181, .T. ) ;
#6495 = DIRECTION ( 'NONE',  ( 1.000000000000000000, -0.000000000000000000, -6.938893903907228378E-17 ) ) ;
#6496 = ORIENTED_EDGE ( 'NONE', *, *, #564, .T. ) ;
#6497 = FACE_OUTER_BOUND ( 'NONE', #5897, .T. ) ;
#6498 = DIRECTION ( 'NONE',  ( -1.159061634649218351E-16, 0.000000000000000000, -1.000000000000000000 ) ) ;
#6499 = ORIENTED_EDGE ( 'NONE', *, *, #6685, .F. ) ;
#6500 = CIRCLE ( 'NONE', #6286, 2.800000000000003819 ) ;
#6501 = DIRECTION ( 'NONE',  ( 1.084202172485504434E-16, 0.000000000000000000, 1.000000000000000000 ) ) ;
#6502 = CARTESIAN_POINT ( 'NONE',  ( 0.000000000000000000, 5.895746314278404121, -2.916892913127026254 ) ) ;
#6503 = CARTESIAN_POINT ( 'NONE',  ( 19.99999999999999645, 0.000000000000000000, 0.000000000000000000 ) ) ;
#6504 = UNCERTAINTY_MEASURE_WITH_UNIT (LENGTH_MEASURE( 1.000000000000000082E-05 ), #3934, 'distance_accuracy_value', 'NONE');
#6505 = LINE ( 'NONE', #6566, #12359 ) ;
#6506 = ORIENTED_EDGE ( 'NONE', *, *, #7176, .F. ) ;
#6507 = ORIENTED_EDGE ( 'NONE', *, *, #5923, .F. ) ;
#6508 = AXIS2_PLACEMENT_3D ( 'NONE', #9011, #3375, #7292 ) ;
#6509 = CARTESIAN_POINT ( 'NONE',  ( 20.00000000000000355, 14.50364731389636397, -24.59751492040896892 ) ) ;
#6510 = CARTESIAN_POINT ( 'NONE',  ( 40.00000000000002842, -19.99999999999997868, -12.00000000000006928 ) ) ;
#6511 = ORIENTED_EDGE ( 'NONE', *, *, #11924, .T. ) ;
#6512 = DIRECTION ( 'NONE',  ( 0.000000000000000000, 0.000000000000000000, 1.000000000000000000 ) ) ;
#6513 = CARTESIAN_POINT ( 'NONE',  ( 19.99999999999997868, 6.496448636052932990, -0.1820882179769736653 ) ) ;
#6514 = AXIS2_PLACEMENT_3D ( 'NONE', #9668, #3713, #4738 ) ;
#6515 = AXIS2_PLACEMENT_3D ( 'NONE', #1383, #9048, #1319 ) ;
#6516 = CARTESIAN_POINT ( 'NONE',  ( 19.99999999999999645, 3.238809497145207494, 5.634457741540175313 ) ) ;
#6517 = LINE ( 'NONE', #6648, #10888 ) ;
#6518 = ORIENTED_EDGE ( 'NONE', *, *, #10714, .T. ) ;
#6519 = DIRECTION ( 'NONE',  ( -4.930380657631325535E-31, -1.000000000000000000, -1.177425296209239362E-30 ) ) ;
#6520 = EDGE_CURVE ( 'NONE', #12630, #2783, #5238, .T. ) ;
#6521 = CARTESIAN_POINT ( 'NONE',  ( 19.99999999999999645, -4.621065432155044839, -4.569765340993108715 ) ) ;
#6522 = ADVANCED_FACE ( 'NONE', ( #2447 ), #10209, .F. ) ;
#6523 = SHAPE_REPRESENTATION_RELATIONSHIP ( 'NONE' , 'NONE' ,  #3471, #4339 ) ;
#6524 = AXIS2_PLACEMENT_3D ( 'NONE', #6398, #10233, #467 ) ;
#6525 = VECTOR ( 'NONE', #7757, 1000.000000000000000 ) ;
#6526 = CARTESIAN_POINT ( 'NONE',  ( 19.99999999999999645, -4.046291478462229030, 5.186098161460289901 ) ) ;
#6527 = ORIENTED_EDGE ( 'NONE', *, *, #5419, .T. ) ;
#6528 = DIRECTION ( 'NONE',  ( -1.000000000000000000, 6.162975822039154730E-33, 4.563833282352349791E-17 ) ) ;
#6529 = EDGE_CURVE ( 'NONE', #7823, #8669, #501, .T. ) ;
#6530 = CARTESIAN_POINT ( 'NONE',  ( -10.00000000000000178, 0.000000000000000000, 0.000000000000000000 ) ) ;
#6531 = CARTESIAN_POINT ( 'NONE',  ( 19.99999999999999645, -4.046291478462170410, -5.186098161460359179 ) ) ;
#6532 = DIRECTION ( 'NONE',  ( -1.000000000000000000, 1.010728034814421376E-30, 1.090846720500930387E-30 ) ) ;
#6533 = DIRECTION ( 'NONE',  ( -1.000000000000000000, 0.000000000000000000, 1.301042606982602363E-16 ) ) ;
#6534 = AXIS2_PLACEMENT_3D ( 'NONE', #700, #12501, #5600 ) ;
#6535 = AXIS2_PLACEMENT_3D ( 'NONE', #2207, #6125, #10034 ) ;
#6536 = DIRECTION ( 'NONE',  ( 0.000000000000000000, 1.000000000000000000, 0.000000000000000000 ) ) ;
#6537 = VECTOR ( 'NONE', #908, 1000.000000000000000 ) ;
#6538 = FACE_OUTER_BOUND ( 'NONE', #5217, .T. ) ;
#6539 = CARTESIAN_POINT ( 'NONE',  ( 4.200000000000001954, 0.000000000000000000, 0.000000000000000000 ) ) ;
#6540 = ORIENTED_EDGE ( 'NONE', *, *, #916, .F. ) ;
#6541 = ORIENTED_EDGE ( 'NONE', *, *, #5344, .T. ) ;
#6542 = VERTEX_POINT ( 'NONE', #9251 ) ;
#6543 = AXIS2_PLACEMENT_3D ( 'NONE', #8610, #12556, #500 ) ;
#6544 = CARTESIAN_POINT ( 'NONE',  ( 19.99999999999999645, 0.000000000000000000, 0.000000000000000000 ) ) ;
#6545 = DIRECTION ( 'NONE',  ( 0.000000000000000000, 1.779758311459930245E-16, 1.000000000000000000 ) ) ;
#6546 = CARTESIAN_POINT ( 'NONE',  ( 14.00000000000000000, -30.00000000000000000, -3.999999999999997335 ) ) ;
#6547 = FACE_OUTER_BOUND ( 'NONE', #2259, .T. ) ;
#6548 = ORIENTED_EDGE ( 'NONE', *, *, #1873, .T. ) ;
#6549 = DIRECTION ( 'NONE',  ( 1.000000000000000000, -6.162975822039154730E-33, -4.563833282352349791E-17 ) ) ;
#6550 = DIRECTION ( 'NONE',  ( -1.000000000000000000, 1.010728034814421376E-30, 1.090846720500930387E-30 ) ) ;
#6551 = ORIENTED_EDGE ( 'NONE', *, *, #3563, .F. ) ;
#6552 = VERTEX_POINT ( 'NONE', #134 ) ;
#6553 = DIRECTION ( 'NONE',  ( -3.437775699846489820E-17, -0.2951046417778627751, -0.9554649393887560960 ) ) ;
#6554 = EDGE_LOOP ( 'NONE', ( #2614, #3276, #5627, #3808 ) ) ;
#6555 = ORIENTED_EDGE ( 'NONE', *, *, #5301, .F. ) ;
#6556 = CARTESIAN_POINT ( 'NONE',  ( 9.000000000000028422, 30.00000000000000000, -5.960102014102692796E-16 ) ) ;
#6557 = ORIENTED_EDGE ( 'NONE', *, *, #7796, .F. ) ;
#6558 = DIRECTION ( 'NONE',  ( 0.000000000000000000, 1.530455820933490821E-32, -1.000000000000000000 ) ) ;
#6559 = CARTESIAN_POINT ( 'NONE',  ( 0.000000000000000000, 1.764426149628130602, 7.186570834724196111 ) ) ;
#6560 = ORIENTED_EDGE ( 'NONE', *, *, #6612, .T. ) ;
#6561 = CARTESIAN_POINT ( 'NONE',  ( 0.3208286057739622166, -4.433571671609698228, -0.3503314178412686997 ) ) ;
#6562 = ADVANCED_FACE ( 'NONE', ( #2513 ), #4209, .T. ) ;
#6563 = DIRECTION ( 'NONE',  ( 0.000000000000000000, 0.000000000000000000, 1.000000000000000000 ) ) ;
#6564 = CIRCLE ( 'NONE', #8394, 1.535500000000000087 ) ;
#6565 = CARTESIAN_POINT ( 'NONE',  ( 0.000000000000000000, -3.426907987218776430, -5.522074125465566752 ) ) ;
#6566 = CARTESIAN_POINT ( 'NONE',  ( -32.14999999999999147, 0.000000000000000000, 3.477184903947654954E-15 ) ) ;
#6567 = VERTEX_POINT ( 'NONE', #9905 ) ;
#6568 = CIRCLE ( 'NONE', #6975, 6.999999999999999112 ) ;
#6569 = ORIENTED_EDGE ( 'NONE', *, *, #1398, .T. ) ;
#6570 = CARTESIAN_POINT ( 'NONE',  ( 19.99999999999997868, 1.395418990828298567, -6.428133065596409068 ) ) ;
#6571 = CARTESIAN_POINT ( 'NONE',  ( 25.00000000000000000, 3.469446951953614189E-14, -1.233886431964027279E-13 ) ) ;
#6572 = ORIENTED_EDGE ( 'NONE', *, *, #3364, .T. ) ;
#6573 = DIRECTION ( 'NONE',  ( 0.000000000000000000, 0.000000000000000000, 1.000000000000000000 ) ) ;
#6574 = DIRECTION ( 'NONE',  ( -1.000000000000000000, 0.000000000000000000, 0.000000000000000000 ) ) ;
#6575 = EDGE_CURVE ( 'NONE', #6747, #3023, #5439, .T. ) ;
#6576 = EDGE_CURVE ( 'NONE', #7990, #11974, #1097, .T. ) ;
#6577 = CIRCLE ( 'NONE', #2460, 2.800000000000004263 ) ;
#6578 = VECTOR ( 'NONE', #11329, 1000.000000000000000 ) ;
#6579 = EDGE_CURVE ( 'NONE', #38, #4694, #2357, .T. ) ;
#6580 = VECTOR ( 'NONE', #11616, 1000.000000000000000 ) ;
#6581 = FACE_OUTER_BOUND ( 'NONE', #7091, .T. ) ;
#6582 = CIRCLE ( 'NONE', #783, 2.800000000000003819 ) ;
#6583 = DIRECTION ( 'NONE',  ( 1.000000000000000000, -1.010728034814421376E-30, -1.090846720500930387E-30 ) ) ;
#6584 = EDGE_LOOP ( 'NONE', ( #4496, #9536, #5767, #9119 ) ) ;
#6585 = CARTESIAN_POINT ( 'NONE',  ( -0.02511973781849641263, 4.877415612947407553, -3.751298745799847456 ) ) ;
#6586 = EDGE_CURVE ( 'NONE', #12298, #11175, #5332, .T. ) ;
#6587 = CARTESIAN_POINT ( 'NONE',  ( -4.101948962586043024, -2.368261337751181639, -3.681124513963744516 ) ) ;
#6588 = AXIS2_PLACEMENT_3D ( 'NONE', #5665, #12509, #4585 ) ;
#6589 = CIRCLE ( 'NONE', #5935, 4.000000000000008882 ) ;
#6590 = DIRECTION ( 'NONE',  ( -9.737501798821850460E-31, 0.9909497617679351444, -0.1342332658176521587 ) ) ;
#6591 =( REPRESENTATION_RELATIONSHIP ('NONE','NONE', #10018, #3471 ) REPRESENTATION_RELATIONSHIP_WITH_TRANSFORMATION ( #7187 )SHAPE_REPRESENTATION_RELATIONSHIP( ) );
#6592 = DIRECTION ( 'NONE',  ( 0.000000000000000000, 0.000000000000000000, 1.000000000000000000 ) ) ;
#6593 = DIRECTION ( 'NONE',  ( -3.266377185680748504E-31, 0.8805955318567392220, -0.4738686624729965824 ) ) ;
#6594 = LINE ( 'NONE', #2675, #11051 ) ;
#6595 = DIRECTION ( 'NONE',  ( 1.000000000000000000, 0.000000000000000000, 0.000000000000000000 ) ) ;
#6596 = DIRECTION ( 'NONE',  ( 0.000000000000000000, 0.000000000000000000, 1.000000000000000000 ) ) ;
#6597 = AXIS2_PLACEMENT_3D ( 'NONE', #2560, #9418, #6485 ) ;
#6598 = AXIS2_PLACEMENT_3D ( 'NONE', #6425, #1583, #12053 ) ;
#6599 = AXIS2_PLACEMENT_3D ( 'NONE', #8706, #2989, #1030 ) ;
#6600 = CARTESIAN_POINT ( 'NONE',  ( 0.000000000000000000, -6.133480037816475772, -2.376659734729558160 ) ) ;
#6601 = PRODUCT ( 'cover 1', 'cover 1', '', ( #7059 ) ) ;
#6602 = CARTESIAN_POINT ( 'NONE',  ( 14.00000000000000000, 30.00000000000000000, 0.000000000000000000 ) ) ;
#6603 = UNCERTAINTY_MEASURE_WITH_UNIT (LENGTH_MEASURE( 1.000000000000000082E-05 ), #1565, 'distance_accuracy_value', 'NONE');
#6604 = EDGE_CURVE ( 'NONE', #10994, #6460, #2154, .T. ) ;
#6605 = CARTESIAN_POINT ( 'NONE',  ( 19.99999999999999645, 0.000000000000000000, 0.000000000000000000 ) ) ;
#6606 = ORIENTED_EDGE ( 'NONE', *, *, #10578, .F. ) ;
#6607 = ORIENTED_EDGE ( 'NONE', *, *, #9917, .T. ) ;
#6608 = EDGE_LOOP ( 'NONE', ( #557, #12046, #10932, #4052 ) ) ;
#6609 = CYLINDRICAL_SURFACE ( 'NONE', #12003, 7.999999999999998224 ) ;
#6610 = DIRECTION ( 'NONE',  ( -1.000000000000000000, 1.010728034814421376E-30, 1.090846720500930387E-30 ) ) ;
#6611 = CYLINDRICAL_SURFACE ( 'NONE', #12329, 6.000000000000013323 ) ;
#6612 = EDGE_CURVE ( 'NONE', #12136, #7823, #11267, .T. ) ;
#6613 = CYLINDRICAL_SURFACE ( 'NONE', #3834, 2.499999999999990230 ) ;
#6614 = ORIENTED_EDGE ( 'NONE', *, *, #9073, .T. ) ;
#6615 = EDGE_CURVE ( 'NONE', #3169, #1463, #7401, .T. ) ;
#6616 = DIRECTION ( 'NONE',  ( -1.000000000000000000, 1.010728034814421376E-30, 1.090846720500930387E-30 ) ) ;
#6617 = PRESENTATION_LAYER_ASSIGNMENT (  '', '', ( #8033 ) ) ;
#6618 =( NAMED_UNIT ( * ) PLANE_ANGLE_UNIT ( ) SI_UNIT ( $, .RADIAN. ) );
#6619 = VERTEX_POINT ( 'NONE', #570 ) ;
#6620 = ORIENTED_EDGE ( 'NONE', *, *, #10728, .F. ) ;
#6621 = DIRECTION ( 'NONE',  ( 0.000000000000000000, -0.000000000000000000, 1.000000000000000000 ) ) ;
#6622 = VERTEX_POINT ( 'NONE', #5465 ) ;
#6623 = ORIENTED_EDGE ( 'NONE', *, *, #8111, .T. ) ;
#6624 = DIRECTION ( 'NONE',  ( 0.000000000000000000, -0.5000000000000011102, -0.8660254037844379305 ) ) ;
#6625 = CARTESIAN_POINT ( 'NONE',  ( 19.99999999999997868, -0.8135880386782390339, -6.527339685683426929 ) ) ;
#6626 = VERTEX_POINT ( 'NONE', #9373 ) ;
#6627 = LINE ( 'NONE', #10537, #7185 ) ;
#6628 = DIRECTION ( 'NONE',  ( 0.000000000000000000, -1.000000000000000000, 0.000000000000000000 ) ) ;
#6629 = AXIS2_PLACEMENT_3D ( 'NONE', #4152, #157, #9930 ) ;
#6630 = EDGE_LOOP ( 'NONE', ( #9499, #11510 ) ) ;
#6631 = DIRECTION ( 'NONE',  ( 0.000000000000000000, 0.000000000000000000, 1.000000000000000000 ) ) ;
#6632 = DIRECTION ( 'NONE',  ( 1.140150527077241873E-30, 0.000000000000000000, -1.000000000000000000 ) ) ;
#6633 = EDGE_CURVE ( 'NONE', #6983, #8089, #3801, .T. ) ;
#6634 = UNCERTAINTY_MEASURE_WITH_UNIT (LENGTH_MEASURE( 1.000000000000000082E-05 ), #10560, 'distance_accuracy_value', 'NONE');
#6635 = EDGE_CURVE ( 'NONE', #9579, #11818, #11832, .T. ) ;
#6636 = VERTEX_POINT ( 'NONE', #12494 ) ;
#6637 = CIRCLE ( 'NONE', #4363, 2.800000000000003819 ) ;
#6638 = ORIENTED_EDGE ( 'NONE', *, *, #4317, .F. ) ;
#6639 = DIRECTION ( 'NONE',  ( 0.000000000000000000, 0.000000000000000000, -1.000000000000000000 ) ) ;
#6640 = DIRECTION ( 'NONE',  ( 1.000000000000000000, 0.000000000000000000, 0.000000000000000000 ) ) ;
#6641 = ORIENTED_EDGE ( 'NONE', *, *, #5646, .F. ) ;
#6642 = LINE ( 'NONE', #9447, #6379 ) ;
#6643 = CLOSED_SHELL ( 'NONE', ( #8273, #11544, #3922, #8299, #10085, #5105, #948, #220, #7496, #5278, #10403, #367, #7416, #5690, #6864, #12661, #2727, #11484, #10191, #10012, #6915, #2193, #4281, #12268, #11122, #10355, #5934, #10526, #7711, #9846, #3620, #8053, #4521, #615 ) ) ;
#6644 = DIRECTION ( 'NONE',  ( 0.000000000000000000, 0.000000000000000000, -1.000000000000000000 ) ) ;
#6645 = VECTOR ( 'NONE', #11014, 1000.000000000000000 ) ;
#6646 = EDGE_CURVE ( 'NONE', #9518, #10853, #5650, .T. ) ;
#6647 = FACE_OUTER_BOUND ( 'NONE', #8663, .T. ) ;
#6648 = CARTESIAN_POINT ( 'NONE',  ( 9.000000000000035527, 30.00000000000000000, 25.00000000000007105 ) ) ;
#6649 = ORIENTED_EDGE ( 'NONE', *, *, #5855, .T. ) ;
#6650 = DIRECTION ( 'NONE',  ( 0.000000000000000000, 1.000000000000000000, 0.000000000000000000 ) ) ;
#6651 = ORIENTED_EDGE ( 'NONE', *, *, #9381, .T. ) ;
#6652 = LINE ( 'NONE', #3562, #10309 ) ;
#6653 = EDGE_CURVE ( 'NONE', #12092, #7976, #4570, .T. ) ;
#6654 = CIRCLE ( 'NONE', #1904, 6.499000000000008548 ) ;
#6655 = EDGE_CURVE ( 'NONE', #9867, #5057, #11622, .T. ) ;
#6656 =( LENGTH_UNIT ( ) NAMED_UNIT ( * ) SI_UNIT ( .MILLI., .METRE. ) );
#6657 = CARTESIAN_POINT ( 'NONE',  ( 33.00000000000000000, 32.50906206197875292, -8.925292473609250266 ) ) ;
#6658 = LINE ( 'NONE', #13, #3743 ) ;
#6659 = FACE_OUTER_BOUND ( 'NONE', #745, .T. ) ;
#6660 = AXIS2_PLACEMENT_3D ( 'NONE', #7714, #11700, #5771 ) ;
#6661 = CARTESIAN_POINT ( 'NONE',  ( 19.99999999999999645, -5.932103089875941038, 2.654647609586679113 ) ) ;
#6662 = DIRECTION ( 'NONE',  ( -1.380506584136768733E-30, 0.4338837391175525693, 0.9009688679024219216 ) ) ;
#6663 = FACE_OUTER_BOUND ( 'NONE', #4237, .T. ) ;
#6664 = CARTESIAN_POINT ( 'NONE',  ( 20.00000000000006750, -8.724036641233686229E-16, -20.00000000000000000 ) ) ;
#6665 =( NAMED_UNIT ( * ) PLANE_ANGLE_UNIT ( ) SI_UNIT ( $, .RADIAN. ) );
#6666 = CARTESIAN_POINT ( 'NONE',  ( 19.99999999999997868, 2.649444137877677186, -6.020675595748665287 ) ) ;
#6667 = VERTEX_POINT ( 'NONE', #756 ) ;
#6668 = PRODUCT_RELATED_PRODUCT_CATEGORY ( 'part', '', ( #12041 ) ) ;
#6669 = EDGE_LOOP ( 'NONE', ( #12670, #3714, #12419, #3719 ) ) ;
#6670 = ORIENTED_EDGE ( 'NONE', *, *, #12134, .T. ) ;
#6671 = DIRECTION ( 'NONE',  ( -1.000000000000000000, 1.010728034814421376E-30, 1.090846720500930387E-30 ) ) ;
#6672 = DIRECTION ( 'NONE',  ( -1.000000000000000000, 1.010728034814421376E-30, 1.090846720500930387E-30 ) ) ;
#6673 = CARTESIAN_POINT ( 'NONE',  ( -35.00000000000006395, -2.157041537713704155E-29, 2.168404344971033323E-15 ) ) ;
#6674 = CARTESIAN_POINT ( 'NONE',  ( 19.99999999999999645, -6.182645281642477286, -2.245659411033190445 ) ) ;
#6675 = VERTEX_POINT ( 'NONE', #7582 ) ;
#6676 = ADVANCED_FACE ( 'NONE', ( #2844 ), #1786, .T. ) ;
#6677 = CARTESIAN_POINT ( 'NONE',  ( 9.999999999999998224, -2.401522331692811818, -6.999477872697428715 ) ) ;
#6678 = AXIS2_PLACEMENT_3D ( 'NONE', #5269, #4178, #4369 ) ;
#6679 = CARTESIAN_POINT ( 'NONE',  ( 11.00000000000003020, -30.00000000000000000, 5.000000000000011546 ) ) ;
#6680 = ORIENTED_EDGE ( 'NONE', *, *, #3070, .F. ) ;
#6681 = ORIENTED_EDGE ( 'NONE', *, *, #894, .F. ) ;
#6682 = DIRECTION ( 'NONE',  ( 1.084202172485504434E-16, 0.000000000000000000, 1.000000000000000000 ) ) ;
#6683 = EDGE_LOOP ( 'NONE', ( #823, #11143, #2947, #11222 ) ) ;
#6684 = VERTEX_POINT ( 'NONE', #7717 ) ;
#6685 = EDGE_CURVE ( 'NONE', #4490, #9929, #3411, .T. ) ;
#6686 = AXIS2_PLACEMENT_3D ( 'NONE', #2017, #4926, #6866 ) ;
#6687 = EDGE_CURVE ( 'NONE', #12468, #2451, #9623, .T. ) ;
#6688 = DIRECTION ( 'NONE',  ( -1.000000000000000000, 1.010728034814421376E-30, 1.090846720500930387E-30 ) ) ;
#6689 = ORIENTED_EDGE ( 'NONE', *, *, #8242, .F. ) ;
#6690 = EDGE_CURVE ( 'NONE', #5492, #11154, #12035, .T. ) ;
#6691 = PLANE ( 'NONE',  #12736 ) ;
#6692 = CARTESIAN_POINT ( 'NONE',  ( 27.00000000000001421, 39.34792583643766761, -17.06347054209568270 ) ) ;
#6693 = ORIENTED_EDGE ( 'NONE', *, *, #12515, .T. ) ;
#6694 = DIRECTION ( 'NONE',  ( -1.000000000000000000, -5.916456789157575403E-31, -2.465190328815656418E-32 ) ) ;
#6695 = ADVANCED_FACE ( 'NONE', ( #2577 ), #7653, .T. ) ;
#6696 = CARTESIAN_POINT ( 'NONE',  ( 6.000000000000000000, 49.63999999999998636, -5.000000000000000888 ) ) ;
#6697 = CIRCLE ( 'NONE', #4421, 2.200000000000003730 ) ;
#6698 = ORIENTED_EDGE ( 'NONE', *, *, #10875, .F. ) ;
#6699 = ORIENTED_EDGE ( 'NONE', *, *, #2647, .F. ) ;
#6700 = CYLINDRICAL_SURFACE ( 'NONE', #5400, 2.800000000000003819 ) ;
#6701 = VECTOR ( 'NONE', #4504, 1000.000000000000000 ) ;
#6702 = DIRECTION ( 'NONE',  ( -1.000000000000000000, -1.081682119347362869E-16, 3.143182988685428759E-16 ) ) ;
#6703 = ORIENTED_EDGE ( 'NONE', *, *, #382, .F. ) ;
#6704 = VECTOR ( 'NONE', #9942, 1000.000000000000000 ) ;
#6705 = DIRECTION ( 'NONE',  ( -1.000000000000000000, 1.010728034814421376E-30, 1.090846720500930387E-30 ) ) ;
#6706 = DIRECTION ( 'NONE',  ( 6.938893903907224680E-17, -3.250006781153453386E-32, 1.000000000000000000 ) ) ;
#6707 = DIRECTION ( 'NONE',  ( -1.140150527077241873E-30, 0.000000000000000000, 1.000000000000000000 ) ) ;
#6708 = CIRCLE ( 'NONE', #1960, 9.999999999999998224 ) ;
#6709 = DIRECTION ( 'NONE',  ( 2.218671295934093250E-30, -5.551115123125776539E-17, -1.000000000000000000 ) ) ;
#6710 = ORIENTED_EDGE ( 'NONE', *, *, #10574, .F. ) ;
#6711 = CARTESIAN_POINT ( 'NONE',  ( 20.00000000000000000, 10.63631887905125950, -9.927230231572497843 ) ) ;
#6712 = ORIENTED_EDGE ( 'NONE', *, *, #11725, .F. ) ;
#6713 = DIRECTION ( 'NONE',  ( -1.154721252774410589E-34, -3.250006781153453386E-32, 1.000000000000000000 ) ) ;
#6714 = SURFACE_STYLE_FILL_AREA ( #5612 ) ;
#6715 = DIRECTION ( 'NONE',  ( -3.437775699846489820E-17, -0.2951046417778627751, -0.9554649393887560960 ) ) ;
#6716 = PLANE ( 'NONE',  #2938 ) ;
#6717 =( GEOMETRIC_REPRESENTATION_CONTEXT ( 3 ) GLOBAL_UNCERTAINTY_ASSIGNED_CONTEXT ( ( #10698 ) ) GLOBAL_UNIT_ASSIGNED_CONTEXT ( ( #9365, #10470, #5522 ) ) REPRESENTATION_CONTEXT ( 'NONE', 'WORKASPACE' ) );
#6718 = DIRECTION ( 'NONE',  ( 0.000000000000000000, 0.000000000000000000, 1.000000000000000000 ) ) ;
#6719 = CARTESIAN_POINT ( 'NONE',  ( -10.00000000000000178, 0.000000000000000000, 0.000000000000000000 ) ) ;
#6720 = CARTESIAN_POINT ( 'NONE',  ( 32.99999999999999289, 39.34792583643766051, -17.06347054209567915 ) ) ;
#6721 = EDGE_CURVE ( 'NONE', #3292, #9808, #6895, .T. ) ;
#6722 = CARTESIAN_POINT ( 'NONE',  ( -11.83215956619923226, 30.00000000000000000, -2.000000000000000888 ) ) ;
#6723 = LINE ( 'NONE', #10445, #2988 ) ;
#6724 = CARTESIAN_POINT ( 'NONE',  ( 19.99999999999999645, 0.000000000000000000, 0.000000000000000000 ) ) ;
#6725 = AXIS2_PLACEMENT_3D ( 'NONE', #9294, #485, #2496 ) ;
#6726 = AXIS2_PLACEMENT_3D ( 'NONE', #12534, #7563, #3709 ) ;
#6727 = DIRECTION ( 'NONE',  ( -1.000000000000000000, 1.010728034814421376E-30, 1.090846720500930387E-30 ) ) ;
#6728 = VERTEX_POINT ( 'NONE', #692 ) ;
#6729 = VERTEX_POINT ( 'NONE', #11587 ) ;
#6730 = DIRECTION ( 'NONE',  ( 1.725633230170963324E-31, 1.000000000000000000, -1.982541115402070533E-16 ) ) ;
#6731 = DIRECTION ( 'NONE',  ( 0.000000000000000000, 0.000000000000000000, 1.000000000000000000 ) ) ;
#6732 = CARTESIAN_POINT ( 'NONE',  ( -10.00000000000000178, 0.000000000000000000, 0.000000000000000000 ) ) ;
#6733 = CIRCLE ( 'NONE', #10415, 2.800000000000002043 ) ;
#6734 = CARTESIAN_POINT ( 'NONE',  ( 19.99999999999999645, -5.932103089875909951, -2.654647609586772816 ) ) ;
#6735 = EDGE_LOOP ( 'NONE', ( #6831, #473, #1133, #8155, #9349 ) ) ;
#6736 = AXIS2_PLACEMENT_3D ( 'NONE', #12205, #4268, #2348 ) ;
#6737 = FACE_BOUND ( 'NONE', #5209, .T. ) ;
#6738 = EDGE_CURVE ( 'NONE', #12468, #2127, #3790, .T. ) ;
#6739 = SURFACE_STYLE_USAGE ( .BOTH. , #1832 ) ;
#6740 = VERTEX_POINT ( 'NONE', #11526 ) ;
#6741 = ORIENTED_EDGE ( 'NONE', *, *, #2921, .T. ) ;
#6742 = CARTESIAN_POINT ( 'NONE',  ( 19.99999999999997868, 6.544726022087268724, -0.6592800351836389794 ) ) ;
#6743 = EDGE_LOOP ( 'NONE', ( #4407, #10089, #6335, #4044 ) ) ;
#6744 = ORIENTED_EDGE ( 'NONE', *, *, #9688, .F. ) ;
#6745 = CIRCLE ( 'NONE', #1381, 2.500000000000000444 ) ;
#6746 = DIRECTION ( 'NONE',  ( 0.000000000000000000, 1.000000000000000000, 0.000000000000000000 ) ) ;
#6747 = VERTEX_POINT ( 'NONE', #2716 ) ;
#6748 = DIRECTION ( 'NONE',  ( -2.218671295934093601E-30, 5.551115123125776539E-17, 1.000000000000000000 ) ) ;
#6749 = CARTESIAN_POINT ( 'NONE',  ( 20.00000000000006750, -8.724036641233686229E-16, -20.00000000000000000 ) ) ;
#6750 = ORIENTED_EDGE ( 'NONE', *, *, #10964, .T. ) ;
#6751 = DIRECTION ( 'NONE',  ( 1.000000000000000000, 0.000000000000000000, 0.000000000000000000 ) ) ;
#6752 = FACE_OUTER_BOUND ( 'NONE', #5139, .T. ) ;
#6753 = EDGE_CURVE ( 'NONE', #11058, #8301, #2996, .T. ) ;
#6754 = EDGE_CURVE ( 'NONE', #10338, #2848, #631, .T. ) ;
#6755 = ORIENTED_EDGE ( 'NONE', *, *, #9809, .T. ) ;
#6756 = ORIENTED_EDGE ( 'NONE', *, *, #2921, .F. ) ;
#6757 = ORIENTED_EDGE ( 'NONE', *, *, #4894, .F. ) ;
#6758 = DIRECTION ( 'NONE',  ( -1.000000000000000000, 1.010728034814421376E-30, 1.090846720500930387E-30 ) ) ;
#6759 = ADVANCED_FACE ( 'NONE', ( #6752 ), #10661, .F. ) ;
#6760 = ORIENTED_EDGE ( 'NONE', *, *, #7518, .T. ) ;
#6761 = DIRECTION ( 'NONE',  ( 0.000000000000000000, 0.000000000000000000, -1.000000000000000000 ) ) ;
#6762 = VECTOR ( 'NONE', #6924, 1000.000000000000000 ) ;
#6763 = ORIENTED_EDGE ( 'NONE', *, *, #8875, .T. ) ;
#6764 = DIRECTION ( 'NONE',  ( 1.000000000000000000, -6.162975822039154730E-33, -4.563833282352349791E-17 ) ) ;
#6765 = EDGE_CURVE ( 'NONE', #6626, #1327, #10580, .T. ) ;
#6766 = EDGE_CURVE ( 'NONE', #10646, #3671, #5528, .T. ) ;
#6767 = CARTESIAN_POINT ( 'NONE',  ( 10.00000000000000000, 49.63999999999998636, -5.000000000000000888 ) ) ;
#6768 = LINE ( 'NONE', #2057, #12143 ) ;
#6769 = EDGE_LOOP ( 'NONE', ( #6423, #1361 ) ) ;
#6770 = CIRCLE ( 'NONE', #5529, 6.499000000000009436 ) ;
#6771 = CARTESIAN_POINT ( 'NONE',  ( 28.99999999999999645, 3.577242133134013559E-15, -1.610000000000001874 ) ) ;
#6772 = ORIENTED_EDGE ( 'NONE', *, *, #10226, .T. ) ;
#6773 = CYLINDRICAL_SURFACE ( 'NONE', #11150, 3.500000000000000000 ) ;
#6774 = SURFACE_STYLE_USAGE ( .BOTH. , #12706 ) ;
#6775 = DIRECTION ( 'NONE',  ( -4.930380657631325535E-31, -1.000000000000000000, -1.177425296209239362E-30 ) ) ;
#6776 = AXIS2_PLACEMENT_3D ( 'NONE', #11279, #11996, #6316 ) ;
#6777 = AXIS2_PLACEMENT_3D ( 'NONE', #57, #8687, #2916 ) ;
#6778 = AXIS2_PLACEMENT_3D ( 'NONE', #2681, #4602, #11680 ) ;
#6779 = CARTESIAN_POINT ( 'NONE',  ( 19.99999999999997868, -1.268072931708450257, -6.374087545670231947 ) ) ;
#6780 = DIRECTION ( 'NONE',  ( -1.000000000000000000, 1.010728034814421376E-30, 1.090846720500930387E-30 ) ) ;
#6781 = CIRCLE ( 'NONE', #11705, 6.000000000000000888 ) ;
#6782 = LINE ( 'NONE', #10817, #9384 ) ;
#6783 = CARTESIAN_POINT ( 'NONE',  ( 3.122502256758252770E-14, -4.862606272033112909, -3.745885042887444616 ) ) ;
#6784 = CARTESIAN_POINT ( 'NONE',  ( -14.99999999999999289, 30.00000000000000000, 25.00000000000007105 ) ) ;
#6785 = DIRECTION ( 'NONE',  ( 0.000000000000000000, -0.9510565162951500895, -0.3090169943749582759 ) ) ;
#6786 = EDGE_CURVE ( 'NONE', #3356, #10646, #1126, .T. ) ;
#6787 = DIRECTION ( 'NONE',  ( 1.000000000000000000, 0.000000000000000000, 0.000000000000000000 ) ) ;
#6788 = VECTOR ( 'NONE', #4183, 1000.000000000000000 ) ;
#6789 = AXIS2_PLACEMENT_3D ( 'NONE', #7685, #785, #6787 ) ;
#6790 = AXIS2_PLACEMENT_3D ( 'NONE', #1841, #9807, #7709 ) ;
#6791 = DIRECTION ( 'NONE',  ( 1.848892746611746419E-31, 1.000000000000000000, -3.250006781153460502E-32 ) ) ;
#6792 = ADVANCED_FACE ( 'NONE', ( #1136 ), #4945, .T. ) ;
#6793 = VERTEX_POINT ( 'NONE', #5905 ) ;
#6794 = ORIENTED_EDGE ( 'NONE', *, *, #8131, .T. ) ;
#6795 = DIRECTION ( 'NONE',  ( -1.000000000000000000, 1.010728034814421376E-30, 1.090846720500930387E-30 ) ) ;
#6796 = AXIS2_PLACEMENT_3D ( 'NONE', #1709, #5635, #2626 ) ;
#6797 = CARTESIAN_POINT ( 'NONE',  ( 20.00000000000000000, 8.901672616175321906, -15.56445005073997301 ) ) ;
#6798 = DIRECTION ( 'NONE',  ( 1.000000000000000000, 1.081682119347366197E-16, -6.938893903907228378E-17 ) ) ;
#6799 = AXIS2_PLACEMENT_3D ( 'NONE', #11479, #6650, #5485 ) ;
#6800 = CIRCLE ( 'NONE', #7000, 2.800000000000003375 ) ;
#6801 = DIRECTION ( 'NONE',  ( 1.000000000000000000, 5.916456789157575403E-31, -1.224646799147352714E-16 ) ) ;
#6802 = EDGE_LOOP ( 'NONE', ( #10083, #12703, #2024, #3094 ) ) ;
#6803 = CARTESIAN_POINT ( 'NONE',  ( -17.00000000000000000, 30.00000000000000000, 3.000000000000030198 ) ) ;
#6804 = DIRECTION ( 'NONE',  ( 1.000000000000000000, 1.849040895279789448E-31, -6.938893903907224680E-17 ) ) ;
#6805 = LINE ( 'NONE', #9485, #2063 ) ;
#6806 = ORIENTED_EDGE ( 'NONE', *, *, #8317, .F. ) ;
#6807 = EDGE_LOOP ( 'NONE', ( #7223, #1569, #10597, #4557 ) ) ;
#6808 = DIRECTION ( 'NONE',  ( 0.000000000000000000, 0.9554649393887557629, -0.2951046417778634412 ) ) ;
#6809 = EDGE_LOOP ( 'NONE', ( #2964, #6290, #11253, #3175, #8753, #10302 ) ) ;
#6810 =( GEOMETRIC_REPRESENTATION_CONTEXT ( 3 ) GLOBAL_UNCERTAINTY_ASSIGNED_CONTEXT ( ( #8653 ) ) GLOBAL_UNIT_ASSIGNED_CONTEXT ( ( #280, #5116, #3206 ) ) REPRESENTATION_CONTEXT ( 'NONE', 'WORKASPACE' ) );
#6811 = EDGE_LOOP ( 'NONE', ( #8139, #1065, #6295, #9674 ) ) ;
#6812 = SURFACE_STYLE_USAGE ( .BOTH. , #4067 ) ;
#6813 = ADVANCED_FACE ( 'NONE', ( #2907 ), #9815, .T. ) ;
#6814 = EDGE_CURVE ( 'NONE', #9943, #490, #6061, .T. ) ;
#6815 = DIRECTION ( 'NONE',  ( -1.000000000000000000, 1.010728034814421376E-30, 1.090846720500930387E-30 ) ) ;
#6816 = EDGE_CURVE ( 'NONE', #6322, #7420, #514, .T. ) ;
#6817 = EDGE_LOOP ( 'NONE', ( #7221, #4545, #544, #2983 ) ) ;
#6818 = DIRECTION ( 'NONE',  ( 0.000000000000000000, 1.000000000000000000, 0.000000000000000000 ) ) ;
#6819 = FACE_OUTER_BOUND ( 'NONE', #12166, .T. ) ;
#6820 = VERTEX_POINT ( 'NONE', #2175 ) ;
#6821 = PLANE ( 'NONE',  #1179 ) ;
#6822 = DIRECTION ( 'NONE',  ( 0.000000000000000000, 0.000000000000000000, 1.000000000000000000 ) ) ;
#6823 = VERTEX_POINT ( 'NONE', #170 ) ;
#6824 = ORIENTED_EDGE ( 'NONE', *, *, #10672, .T. ) ;
#6825 = EDGE_LOOP ( 'NONE', ( #497, #6332 ) ) ;
#6826 = CARTESIAN_POINT ( 'NONE',  ( 12.94787914004603202, 30.00000000000000000, 5.638155724715463890 ) ) ;
#6827 = AXIS2_PLACEMENT_3D ( 'NONE', #6472, #12337, #2612 ) ;
#6828 = ADVANCED_FACE ( 'NONE', ( #7840 ), #2966, .T. ) ;
#6829 = VERTEX_POINT ( 'NONE', #3916 ) ;
#6830 = DIRECTION ( 'NONE',  ( 9.367723249499501176E-31, -0.9989930665413151445, 0.04486483035050446017 ) ) ;
#6831 = ORIENTED_EDGE ( 'NONE', *, *, #12590, .T. ) ;
#6832 = LINE ( 'NONE', #767, #3704 ) ;
#6833 = AXIS2_PLACEMENT_3D ( 'NONE', #11475, #7415, #3621 ) ;
#6834 = EDGE_CURVE ( 'NONE', #8908, #1778, #9342, .T. ) ;
#6835 = CARTESIAN_POINT ( 'NONE',  ( 1.257172072275555497, -3.892973519170928043, -3.433252694550785300 ) ) ;
#6836 = VECTOR ( 'NONE', #9018, 999.9999999999998863 ) ;
#6837 = CARTESIAN_POINT ( 'NONE',  ( 4.200000000000001954, 0.000000000000000000, -1.734723475976807094E-14 ) ) ;
#6838 = APPLICATION_CONTEXT ( 'automotive_design' ) ;
#6839 = ORIENTED_EDGE ( 'NONE', *, *, #11467, .T. ) ;
#6840 = CYLINDRICAL_SURFACE ( 'NONE', #10493, 2.800000000000003819 ) ;
#6841 = ORIENTED_EDGE ( 'NONE', *, *, #838, .T. ) ;
#6842 = DIRECTION ( 'NONE',  ( 2.218671295934093250E-30, -5.551115123125776539E-17, -1.000000000000000000 ) ) ;
#6843 = EDGE_CURVE ( 'NONE', #927, #3906, #7095, .T. ) ;
#6844 = DIRECTION ( 'NONE',  ( -1.000000000000000000, 1.010728034814421376E-30, 1.090846720500930387E-30 ) ) ;
#6845 = CIRCLE ( 'NONE', #4988, 6.499000000000009436 ) ;
#6846 = EDGE_CURVE ( 'NONE', #8089, #2832, #107, .T. ) ;
#6847 = CARTESIAN_POINT ( 'NONE',  ( -31.74999999999995026, 0.000000000000000000, 1.999999999999983569 ) ) ;
#6848 = CARTESIAN_POINT ( 'NONE',  ( 19.99999999999997868, 4.494880553659097444, -4.802513683199186367 ) ) ;
#6849 = LINE ( 'NONE', #2676, #5695 ) ;
#6850 = CARTESIAN_POINT ( 'NONE',  ( 19.99999999999999645, -1.268072931708538853, 6.374087545670210631 ) ) ;
#6851 = DIRECTION ( 'NONE',  ( 1.140150527077241873E-30, 0.000000000000000000, -1.000000000000000000 ) ) ;
#6852 = CIRCLE ( 'NONE', #6224, 14.99999999999998934 ) ;
#6853 = CIRCLE ( 'NONE', #1284, 2.800000000000004263 ) ;
#6854 = DIRECTION ( 'NONE',  ( -0.000000000000000000, -1.000000000000000000, -0.000000000000000000 ) ) ;
#6855 = CYLINDRICAL_SURFACE ( 'NONE', #10928, 6.000000000000000000 ) ;
#6856 = ORIENTED_EDGE ( 'NONE', *, *, #964, .F. ) ;
#6857 = VERTEX_POINT ( 'NONE', #5841 ) ;
#6858 = CARTESIAN_POINT ( 'NONE',  ( 0.000000000000000000, 0.2252065540229633012, 6.573992004634855668 ) ) ;
#6859 =( GEOMETRIC_REPRESENTATION_CONTEXT ( 3 ) GLOBAL_UNCERTAINTY_ASSIGNED_CONTEXT ( ( #3638 ) ) GLOBAL_UNIT_ASSIGNED_CONTEXT ( ( #10533, #10401, #7644 ) ) REPRESENTATION_CONTEXT ( 'NONE', 'WORKASPACE' ) );
#6860 = CARTESIAN_POINT ( 'NONE',  ( -30.00000000000000000, 30.00000000000000000, 2.000000000000001776 ) ) ;
#6861 = CYLINDRICAL_SURFACE ( 'NONE', #993, 6.000000000000000888 ) ;
#6862 = LINE ( 'NONE', #6734, #10188 ) ;
#6863 = VERTEX_POINT ( 'NONE', #9753 ) ;
#6864 = ADVANCED_FACE ( 'NONE', ( #6945, #11970, #10791 ), #9880, .F. ) ;
#6865 = FACE_OUTER_BOUND ( 'NONE', #417, .T. ) ;
#6866 = DIRECTION ( 'NONE',  ( 0.000000000000000000, 5.551115123125776539E-17, 1.000000000000000000 ) ) ;
#6867 = CARTESIAN_POINT ( 'NONE',  ( 19.99999999999999645, 3.908107171477180675, 5.192658214849959819 ) ) ;
#6868 = ORIENTED_EDGE ( 'NONE', *, *, #2224, .F. ) ;
#6869 = VECTOR ( 'NONE', #10518, 1000.000000000000000 ) ;
#6870 = EDGE_LOOP ( 'NONE', ( #5384, #5953, #11441, #3345 ) ) ;
#6871 = FACE_OUTER_BOUND ( 'NONE', #8507, .T. ) ;
#6872 = VERTEX_POINT ( 'NONE', #4095 ) ;
#6873 = ORIENTED_EDGE ( 'NONE', *, *, #6329, .T. ) ;
#6874 = SHAPE_DEFINITION_REPRESENTATION ( #8540, #11514 ) ;
#6875 = CARTESIAN_POINT ( 'NONE',  ( 19.99999999999999645, -5.362766118793865111, 3.671204237728611819 ) ) ;
#6876 = ORIENTED_EDGE ( 'NONE', *, *, #5333, .T. ) ;
#6877 = DIRECTION ( 'NONE',  ( -0.000000000000000000, -1.000000000000000000, -0.000000000000000000 ) ) ;
#6878 = DIRECTION ( 'NONE',  ( -1.000000000000000000, 1.010728034814421376E-30, 1.090846720500930387E-30 ) ) ;
#6879 = ORIENTED_EDGE ( 'NONE', *, *, #12643, .T. ) ;
#6880 = VECTOR ( 'NONE', #11423, 1000.000000000000114 ) ;
#6881 = DIRECTION ( 'NONE',  ( -1.000000000000000000, 1.006188713385347367E-17, 3.844790828812615713E-17 ) ) ;
#6882 = DIRECTION ( 'NONE',  ( -1.000000000000000000, 0.000000000000000000, 0.000000000000000000 ) ) ;
#6883 = EDGE_CURVE ( 'NONE', #490, #11656, #10988, .T. ) ;
#6884 = EDGE_CURVE ( 'NONE', #10108, #6684, #8945, .T. ) ;
#6885 = CIRCLE ( 'NONE', #7084, 6.499000000000008548 ) ;
#6886 = EDGE_LOOP ( 'NONE', ( #6507, #835 ) ) ;
#6887 = ORIENTED_EDGE ( 'NONE', *, *, #4790, .T. ) ;
#6888 = EDGE_LOOP ( 'NONE', ( #10544, #8403, #2436, #523 ) ) ;
#6889 = LINE ( 'NONE', #6826, #8892 ) ;
#6890 = PRODUCT_DEFINITION_SHAPE ( 'NONE', 'NONE',  #12764 ) ;
#6891 = EDGE_LOOP ( 'NONE', ( #3148, #8538 ) ) ;
#6892 = CARTESIAN_POINT ( 'NONE',  ( 19.99999999999999645, 0.000000000000000000, 0.000000000000000000 ) ) ;
#6893 = ORIENTED_EDGE ( 'NONE', *, *, #8723, .F. ) ;
#6894 = VECTOR ( 'NONE', #6382, 1000.000000000000000 ) ;
#6895 = CIRCLE ( 'NONE', #1326, 7.400000000000011902 ) ;
#6896 = CARTESIAN_POINT ( 'NONE',  ( -0.1750025118121416035, -4.719839900820628209, -3.469254087858258284 ) ) ;
#6897 = EDGE_CURVE ( 'NONE', #3836, #12298, #8335, .T. ) ;
#6898 = PRODUCT_DEFINITION ( 'UNKNOWN', '', #6946, #3363 ) ;
#6899 = DIRECTION ( 'NONE',  ( 0.000000000000000000, 0.000000000000000000, 1.000000000000000000 ) ) ;
#6900 = VERTEX_POINT ( 'NONE', #1068 ) ;
#6901 = LINE ( 'NONE', #1869, #4936 ) ;
#6902 = VECTOR ( 'NONE', #8939, 1000.000000000000000 ) ;
#6903 = EDGE_LOOP ( 'NONE', ( #379, #4517, #5453, #7913 ) ) ;
#6904 = AXIS2_PLACEMENT_3D ( 'NONE', #4674, #9482, #9416 ) ;
#6905 = CYLINDRICAL_SURFACE ( 'NONE', #4161, 7.400000000000010125 ) ;
#6906 = LINE ( 'NONE', #12, #11325 ) ;
#6907 = DIRECTION ( 'NONE',  ( 1.000000000000000000, -1.010728034814421376E-30, -1.090846720500930387E-30 ) ) ;
#6908 = CYLINDRICAL_SURFACE ( 'NONE', #6313, 7.400000000000010125 ) ;
#6909 = DIRECTION ( 'NONE',  ( -1.000000000000000000, 1.010728034814421376E-30, 1.090846720500930387E-30 ) ) ;
#6910 = AXIS2_PLACEMENT_3D ( 'NONE', #5428, #7490, #10567 ) ;
#6911 = EDGE_CURVE ( 'NONE', #11649, #6322, #5006, .T. ) ;
#6912 = CARTESIAN_POINT ( 'NONE',  ( 33.00000000000001421, 81.84122341717352356, -27.68198508464163510 ) ) ;
#6913 = EDGE_CURVE ( 'NONE', #5654, #7331, #3089, .T. ) ;
#6914 = CARTESIAN_POINT ( 'NONE',  ( -15.00000000000003375, -30.00000000000000000, 3.000000000000029754 ) ) ;
#6915 = ADVANCED_FACE ( 'NONE', ( #9115 ), #10132, .F. ) ;
#6916 = CARTESIAN_POINT ( 'NONE',  ( 19.99999999999997868, 4.772487208025196992, -4.411390579991299354 ) ) ;
#6917 = LINE ( 'NONE', #7986, #1268 ) ;
#6918 = ADVANCED_FACE ( 'NONE', ( #297 ), #6420, .F. ) ;
#6919 = AXIS2_PLACEMENT_3D ( 'NONE', #3374, #7291, #8182 ) ;
#6920 = ORIENTED_EDGE ( 'NONE', *, *, #12200, .F. ) ;
#6921 = ORIENTED_EDGE ( 'NONE', *, *, #10467, .T. ) ;
#6922 = LINE ( 'NONE', #10829, #1724 ) ;
#6923 = LINE ( 'NONE', #6797, #553 ) ;
#6924 = DIRECTION ( 'NONE',  ( -0.5000000000000061062, 0.000000000000000000, 0.8660254037844351549 ) ) ;
#6925 = CARTESIAN_POINT ( 'NONE',  ( 15.00000000000003375, 30.00000000000001776, 6.000000000000013323 ) ) ;
#6926 = ORIENTED_EDGE ( 'NONE', *, *, #143, .F. ) ;
#6927 = DIRECTION ( 'NONE',  ( -4.930380657631325535E-31, -1.000000000000000000, -1.177425296209239362E-30 ) ) ;
#6928 = AXIS2_PLACEMENT_3D ( 'NONE', #2761, #8592, #1891 ) ;
#6929 = DIRECTION ( 'NONE',  ( 1.000000000000000000, -1.010728034814421376E-30, 1.140150527077241873E-30 ) ) ;
#6930 = CIRCLE ( 'NONE', #9576, 2.149999999999999023 ) ;
#6931 = DIRECTION ( 'NONE',  ( -1.000000000000000000, 1.010728034814421376E-30, 1.090846720500930387E-30 ) ) ;
#6932 = ORIENTED_EDGE ( 'NONE', *, *, #4358, .F. ) ;
#6933 = ORIENTED_EDGE ( 'NONE', *, *, #8130, .F. ) ;
#6934 = CARTESIAN_POINT ( 'NONE',  ( 0.000000000000000000, 4.862606272033057841, -3.745885042887454830 ) ) ;
#6935 = ORIENTED_EDGE ( 'NONE', *, *, #8711, .T. ) ;
#6936 = EDGE_LOOP ( 'NONE', ( #11466, #2953, #5106, #9890 ) ) ;
#6937 = FACE_OUTER_BOUND ( 'NONE', #10793, .T. ) ;
#6938 = ORIENTED_EDGE ( 'NONE', *, *, #6579, .T. ) ;
#6939 = AXIS2_PLACEMENT_3D ( 'NONE', #3572, #7550, #7368 ) ;
#6940 = DIRECTION ( 'NONE',  ( 0.000000000000000000, 0.000000000000000000, 1.000000000000000000 ) ) ;
#6941 = VECTOR ( 'NONE', #12458, 1000.000000000000000 ) ;
#6942 = DIRECTION ( 'NONE',  ( -1.000000000000000000, 1.010728034814421376E-30, 1.090846720500930387E-30 ) ) ;
#6943 = ORIENTED_EDGE ( 'NONE', *, *, #11083, .F. ) ;
#6944 = CARTESIAN_POINT ( 'NONE',  ( 2.000000000000001776, -0.8865213383406727043, 1.535500000000009191 ) ) ;
#6945 = FACE_BOUND ( 'NONE', #8992, .T. ) ;
#6946 = PRODUCT_DEFINITION_FORMATION_WITH_SPECIFIED_SOURCE ( 'ANY', '', #2709, .NOT_KNOWN. ) ;
#6947 = EDGE_LOOP ( 'NONE', ( #9302, #3158 ) ) ;
#6948 = CIRCLE ( 'NONE', #12714, 6.499000000000008548 ) ;
#6949 = ORIENTED_EDGE ( 'NONE', *, *, #2005, .T. ) ;
#6950 = ORIENTED_EDGE ( 'NONE', *, *, #2147, .T. ) ;
#6951 = DIRECTION ( 'NONE',  ( -1.000000000000000000, 0.000000000000000000, 0.000000000000000000 ) ) ;
#6952 = CARTESIAN_POINT ( 'NONE',  ( 0.000000000000000000, 4.618802153517012954, -5.000000000000018652 ) ) ;
#6953 = ORIENTED_EDGE ( 'NONE', *, *, #6911, .T. ) ;
#6954 = CARTESIAN_POINT ( 'NONE',  ( 20.00000000000000000, 15.24625277455639072, -6.248133273622503481 ) ) ;
#6955 = ORIENTED_EDGE ( 'NONE', *, *, #1559, .F. ) ;
#6956 = DIRECTION ( 'NONE',  ( -1.000000000000000000, 1.010728034814421376E-30, 1.090846720500930387E-30 ) ) ;
#6957 = CARTESIAN_POINT ( 'NONE',  ( 4.000000000000000000, -2.309401076758522464, -5.000000000000000888 ) ) ;
#6958 = ORIENTED_EDGE ( 'NONE', *, *, #7713, .T. ) ;
#6959 = LINE ( 'NONE', #12702, #8198 ) ;
#6960 = ORIENTED_EDGE ( 'NONE', *, *, #8008, .F. ) ;
#6961 = LINE ( 'NONE', #1930, #7258 ) ;
#6962 = AXIS2_PLACEMENT_3D ( 'NONE', #4163, #1192, #10253 ) ;
#6963 = EDGE_CURVE ( 'NONE', #6343, #6000, #3469, .T. ) ;
#6964 = LINE ( 'NONE', #11923, #1854 ) ;
#6965 = EDGE_CURVE ( 'NONE', #6024, #11591, #4227, .T. ) ;
#6966 = EDGE_CURVE ( 'NONE', #7469, #7997, #11250, .T. ) ;
#6967 = CARTESIAN_POINT ( 'NONE',  ( 0.000000000000000000, 0.000000000000000000, 0.000000000000000000 ) ) ;
#6968 = CARTESIAN_POINT ( 'NONE',  ( 0.000000000000000000, -6.289597356626510205, 3.898841506334508988 ) ) ;
#6969 = CARTESIAN_POINT ( 'NONE',  ( -3.999999999999994671, -2.309401076758511806, -0.4999999999999865663 ) ) ;
#6970 = DIRECTION ( 'NONE',  ( -1.725633230170963324E-31, -1.000000000000000000, 1.982541115402070533E-16 ) ) ;
#6971 = AXIS2_PLACEMENT_3D ( 'NONE', #1826, #10898, #10705 ) ;
#6972 = DIRECTION ( 'NONE',  ( 1.577021341797099039E-16, 1.177425296209237084E-30, 1.000000000000000000 ) ) ;
#6973 = DIRECTION ( 'NONE',  ( 1.000000000000000000, 0.000000000000000000, -6.375108774214761023E-14 ) ) ;
#6974 = DIRECTION ( 'NONE',  ( -0.8191520442889902442, 8.778333957637496424E-33, -0.5735764363510482688 ) ) ;
#6975 = AXIS2_PLACEMENT_3D ( 'NONE', #4806, #8730, #7766 ) ;
#6976 = CIRCLE ( 'NONE', #4092, 2.800000000000003819 ) ;
#6977 =( GEOMETRIC_REPRESENTATION_CONTEXT ( 3 ) GLOBAL_UNCERTAINTY_ASSIGNED_CONTEXT ( ( #12525 ) ) GLOBAL_UNIT_ASSIGNED_CONTEXT ( ( #2366, #8144, #5124 ) ) REPRESENTATION_CONTEXT ( 'NONE', 'WORKASPACE' ) );
#6978 = ORIENTED_EDGE ( 'NONE', *, *, #3848, .T. ) ;
#6979 = VERTEX_POINT ( 'NONE', #1322 ) ;
#6980 = CARTESIAN_POINT ( 'NONE',  ( 32.99999999999999289, 44.40501137213340144, -30.19113521482024964 ) ) ;
#6981 = CARTESIAN_POINT ( 'NONE',  ( 20.00000000000000355, 18.52447679111067913, -16.77732469694377926 ) ) ;
#6982 = DIRECTION ( 'NONE',  ( -1.000000000000000000, 1.010728034814421376E-30, 1.090846720500930387E-30 ) ) ;
#6983 = VERTEX_POINT ( 'NONE', #12097 ) ;
#6984 = CARTESIAN_POINT ( 'NONE',  ( 19.99999999999997868, 6.424561140605085541, 0.9808237102697028309 ) ) ;
#6985 = CIRCLE ( 'NONE', #1424, 4.000000000000000000 ) ;
#6986 = CIRCLE ( 'NONE', #10255, 1.535500000000000087 ) ;
#6987 = CARTESIAN_POINT ( 'NONE',  ( 2.000000000000001776, -0.8865213383406691516, 1.535500000000002085 ) ) ;
#6988 = EDGE_CURVE ( 'NONE', #7688, #222, #11748, .T. ) ;
#6989 = PRODUCT_DEFINITION_SHAPE ( 'NONE', 'NONE',  #12762 ) ;
#6990 = ORIENTED_EDGE ( 'NONE', *, *, #9338, .T. ) ;
#6991 = AXIS2_PLACEMENT_3D ( 'NONE', #7380, #6341, #2429 ) ;
#6992 = VERTEX_POINT ( 'NONE', #11313 ) ;
#6993 = CARTESIAN_POINT ( 'NONE',  ( 0.000000000000000000, 4.618802153516985420, -3.433295621305398893 ) ) ;
#6994 = ORIENTED_EDGE ( 'NONE', *, *, #4503, .F. ) ;
#6995 = ORIENTED_EDGE ( 'NONE', *, *, #4239, .T. ) ;
#6996 = APPLICATION_PROTOCOL_DEFINITION ( 'draft international standard', 'automotive_design', 1998, #12271 ) ;
#6997 = FACE_OUTER_BOUND ( 'NONE', #2973, .T. ) ;
#6998 = AXIS2_PLACEMENT_3D ( 'NONE', #5041, #3188, #8830 ) ;
#6999 = EDGE_LOOP ( 'NONE', ( #1761, #5146, #8028, #1392 ) ) ;
#7000 = AXIS2_PLACEMENT_3D ( 'NONE', #7740, #9652, #4970 ) ;
#7001 = EDGE_CURVE ( 'NONE', #7272, #1090, #1541, .T. ) ;
#7002 = FACE_OUTER_BOUND ( 'NONE', #370, .T. ) ;
#7003 = EDGE_CURVE ( 'NONE', #1053, #3716, #11003, .T. ) ;
#7004 = CYLINDRICAL_SURFACE ( 'NONE', #8293, 6.499000000000010324 ) ;
#7005 = VERTEX_POINT ( 'NONE', #6155 ) ;
#7006 = LINE ( 'NONE', #9114, #10635 ) ;
#7007 =( REPRESENTATION_RELATIONSHIP ('NONE','NONE', #10018, #8378 ) REPRESENTATION_RELATIONSHIP_WITH_TRANSFORMATION ( #5247 )SHAPE_REPRESENTATION_RELATIONSHIP( ) );
#7008 = CARTESIAN_POINT ( 'NONE',  ( 19.99999999999999645, 0.000000000000000000, 0.000000000000000000 ) ) ;
#7009 = PRESENTATION_LAYER_ASSIGNMENT (  '', '', ( #12570 ) ) ;
#7010 = VECTOR ( 'NONE', #5255, 1000.000000000000000 ) ;
#7011 = EDGE_LOOP ( 'NONE', ( #3920, #4898, #682, #1260, #4579 ) ) ;
#7012 = EDGE_LOOP ( 'NONE', ( #6680, #2310, #10799, #3593 ) ) ;
#7013 = ORIENTED_EDGE ( 'NONE', *, *, #9055, .T. ) ;
#7014 = CARTESIAN_POINT ( 'NONE',  ( 0.000000000000000000, 6.359534927042326480, -1.339147681075104845 ) ) ;
#7015 = ADVANCED_FACE ( 'NONE', ( #10258 ), #1514, .T. ) ;
#7016 = CARTESIAN_POINT ( 'NONE',  ( 4.000000000000001776, 2.472263674411383505, -3.687027874309860564 ) ) ;
#7017 = ORIENTED_EDGE ( 'NONE', *, *, #7999, .F. ) ;
#7018 = CARTESIAN_POINT ( 'NONE',  ( 14.00000000000000000, 13.00000000000000000, 0.000000000000000000 ) ) ;
#7019 = PRESENTATION_LAYER_ASSIGNMENT (  '', '', ( #2072 ) ) ;
#7020 = ORIENTED_EDGE ( 'NONE', *, *, #6897, .F. ) ;
#7021 = DIRECTION ( 'NONE',  ( 0.000000000000000000, 0.9510565162951545304, -0.3090169943749445092 ) ) ;
#7022 = ADVANCED_FACE ( 'NONE', ( #9172 ), #10162, .F. ) ;
#7023 = CARTESIAN_POINT ( 'NONE',  ( 19.99999999999999645, 0.000000000000000000, 0.000000000000000000 ) ) ;
#7024 = LINE ( 'NONE', #9003, #2691 ) ;
#7025 = ORIENTED_EDGE ( 'NONE', *, *, #6239, .T. ) ;
#7026 = DIRECTION ( 'NONE',  ( 1.000000000000000000, -6.162975822039154730E-33, -4.563833282352349791E-17 ) ) ;
#7027 = ORIENTED_EDGE ( 'NONE', *, *, #4600, .T. ) ;
#7028 = CARTESIAN_POINT ( 'NONE',  ( 2.000000000000001776, 1.773042676681338303, 0.000000000000000000 ) ) ;
#7029 = FACE_OUTER_BOUND ( 'NONE', #5009, .T. ) ;
#7030 = AXIS2_PLACEMENT_3D ( 'NONE', #2333, #10155, #8045 ) ;
#7031 = FACE_OUTER_BOUND ( 'NONE', #3468, .T. ) ;
#7032 = CIRCLE ( 'NONE', #5788, 2.800000000000003819 ) ;
#7033 = LINE ( 'NONE', #9080, #3255 ) ;
#7034 = CYLINDRICAL_SURFACE ( 'NONE', #6508, 2.000000000000000888 ) ;
#7035 = DIRECTION ( 'NONE',  ( -0.000000000000000000, -1.000000000000000000, -0.000000000000000000 ) ) ;
#7036 = EDGE_CURVE ( 'NONE', #5894, #11074, #7318, .T. ) ;
#7037 = CARTESIAN_POINT ( 'NONE',  ( 33.00000000000001421, 81.84122341717352356, -12.68198508464164931 ) ) ;
#7038 = EDGE_CURVE ( 'NONE', #9690, #11281, #7325, .T. ) ;
#7039 = DIRECTION ( 'NONE',  ( 0.000000000000000000, 0.000000000000000000, -1.000000000000000000 ) ) ;
#7040 = VECTOR ( 'NONE', #11273, 1000.000000000000000 ) ;
#7041 = PRESENTATION_STYLE_ASSIGNMENT (( #870 ) ) ;
#7042 = ORIENTED_EDGE ( 'NONE', *, *, #4520, .F. ) ;
#7043 = CARTESIAN_POINT ( 'NONE',  ( 0.000000000000000000, 0.000000000000000000, 0.000000000000000000 ) ) ;
#7044 = CARTESIAN_POINT ( 'NONE',  ( -2.500000000000000444, -3.438830781974930402E-14, -25.03750572909320837 ) ) ;
#7045 = DIRECTION ( 'NONE',  ( -1.000000000000000000, 1.010728034814421376E-30, 1.090846720500930387E-30 ) ) ;
#7046 = DIRECTION ( 'NONE',  ( 0.000000000000000000, 0.000000000000000000, -1.000000000000000000 ) ) ;
#7047 = CARTESIAN_POINT ( 'NONE',  ( 0.000000000000000000, 0.000000000000000000, 0.000000000000000000 ) ) ;
#7048 = EDGE_LOOP ( 'NONE', ( #173, #98, #10369, #8397 ) ) ;
#7049 = DIRECTION ( 'NONE',  ( 1.140150527077241873E-30, 0.000000000000000000, -1.000000000000000000 ) ) ;
#7050 = CIRCLE ( 'NONE', #7060, 2.800000000000004263 ) ;
#7051 = DIRECTION ( 'NONE',  ( 1.000000000000000000, -6.162975822039154730E-33, -4.563833282352349791E-17 ) ) ;
#7052 = FILL_AREA_STYLE ('',( #11760 ) ) ;
#7053 = ADVANCED_FACE ( 'NONE', ( #6737, #5633, #10524 ), #676, .T. ) ;
#7054 = ORIENTED_EDGE ( 'NONE', *, *, #3531, .T. ) ;
#7055 = CARTESIAN_POINT ( 'NONE',  ( -10.00000000000000178, 0.000000000000000000, 0.000000000000000000 ) ) ;
#7056 = ORIENTED_EDGE ( 'NONE', *, *, #10969, .F. ) ;
#7057 = CIRCLE ( 'NONE', #882, 7.400000000000011902 ) ;
#7058 = ORIENTED_EDGE ( 'NONE', *, *, #154, .T. ) ;
#7059 = PRODUCT_CONTEXT ( 'NONE', #1307, 'mechanical' ) ;
#7060 = AXIS2_PLACEMENT_3D ( 'NONE', #6570, #12438, #827 ) ;
#7061 = LINE ( 'NONE', #10913, #2695 ) ;
#7062 = VERTEX_POINT ( 'NONE', #7568 ) ;
#7063 = DIRECTION ( 'NONE',  ( -1.000000000000000000, 1.010728034814421376E-30, 1.090846720500930387E-30 ) ) ;
#7064 = VERTEX_POINT ( 'NONE', #10459 ) ;
#7065 = CARTESIAN_POINT ( 'NONE',  ( 15.00000000000003375, 30.00000000000001776, -9.742497179615118866E-31 ) ) ;
#7066 = DIRECTION ( 'NONE',  ( -1.848892746611746419E-31, -1.000000000000000000, 3.250006781153460502E-32 ) ) ;
#7067 = CARTESIAN_POINT ( 'NONE',  ( 14.00000000000000000, 13.00000000000000000, 0.000000000000000000 ) ) ;
#7068 = CARTESIAN_POINT ( 'NONE',  ( 20.00000000000000355, 18.52447679111067913, -16.77732469694377926 ) ) ;
#7069 = CIRCLE ( 'NONE', #11174, 2.800000000000003819 ) ;
#7070 = EDGE_LOOP ( 'NONE', ( #53, #2703, #12286, #1250 ) ) ;
#7071 = ADVANCED_FACE ( 'NONE', ( #10647 ), #1645, .T. ) ;
#7072 = EDGE_LOOP ( 'NONE', ( #1523, #1252, #556, #5640 ) ) ;
#7073 = ORIENTED_EDGE ( 'NONE', *, *, #5489, .F. ) ;
#7074 = EDGE_CURVE ( 'NONE', #3160, #4761, #4553, .T. ) ;
#7075 = ORIENTED_EDGE ( 'NONE', *, *, #4910, .T. ) ;
#7076 = CARTESIAN_POINT ( 'NONE',  ( 19.99999999999999645, 1.528443194675403349, 7.240432404259460775 ) ) ;
#7077 = TOROIDAL_SURFACE ( 'NONE', #4186, 2.200000000000001066, 0.2000000000000000111 ) ;
#7078 = CARTESIAN_POINT ( 'NONE',  ( -4.140404888673263173, -2.228338276487473291, -3.686887068327048045 ) ) ;
#7079 = ORIENTED_EDGE ( 'NONE', *, *, #1228, .T. ) ;
#7080 = ADVANCED_FACE ( 'NONE', ( #797 ), #8532, .T. ) ;
#7081 = CARTESIAN_POINT ( 'NONE',  ( 5.384454397937153303, -3.469446951953614189E-15, -4.484454397937126302 ) ) ;
#7082 = VERTEX_POINT ( 'NONE', #12474 ) ;
#7083 = CARTESIAN_POINT ( 'NONE',  ( 0.000000000000000000, -4.707829255731177831, -5.709320773864598131 ) ) ;
#7084 = AXIS2_PLACEMENT_3D ( 'NONE', #6328, #4211, #8264 ) ;
#7085 = DIRECTION ( 'NONE',  ( -1.000000000000000000, 0.000000000000000000, 0.000000000000000000 ) ) ;
#7086 = CIRCLE ( 'NONE', #3392, 2.800000000000002487 ) ;
#7087 = PRODUCT_DEFINITION_CONTEXT ( 'detailed design', #5265, 'design' ) ;
#7088 = DIRECTION ( 'NONE',  ( 0.000000000000000000, 0.000000000000000000, 1.000000000000000000 ) ) ;
#7089 = EDGE_LOOP ( 'NONE', ( #3643, #3612, #3229, #3049 ) ) ;
#7090 = CARTESIAN_POINT ( 'NONE',  ( 2.000000000000001776, 0.000000000000000000, 0.000000000000000000 ) ) ;
#7091 = EDGE_LOOP ( 'NONE', ( #9423, #11226, #949, #6693 ) ) ;
#7092 = DIRECTION ( 'NONE',  ( 1.000000000000000000, -1.010728034814421376E-30, -1.090846720500930387E-30 ) ) ;
#7093 = AXIS2_PLACEMENT_3D ( 'NONE', #8375, #12314, #2463 ) ;
#7094 = FILL_AREA_STYLE ('',( #9774 ) ) ;
#7095 = CIRCLE ( 'NONE', #10591, 4.000000000000000000 ) ;
#7096 = DIRECTION ( 'NONE',  ( -1.000000000000000000, -1.031065855027150586E-29, 2.218671295934095703E-30 ) ) ;
#7097 = DIRECTION ( 'NONE',  ( -1.000000000000000000, -1.081682119347366197E-16, 6.938893903907228378E-17 ) ) ;
#7098 = DIRECTION ( 'NONE',  ( -1.000000000000000000, 1.006188713385347367E-17, 3.844790828812615713E-17 ) ) ;
#7099 = CARTESIAN_POINT ( 'NONE',  ( 11.00000000000001243, -12.50000000000000000, -6.000000000000017764 ) ) ;
#7100 = AXIS2_PLACEMENT_3D ( 'NONE', #3238, #11335, #9504 ) ;
#7101 = VECTOR ( 'NONE', #10902, 1000.000000000000227 ) ;
#7102 = DIRECTION ( 'NONE',  ( -1.081682119347366321E-16, 1.000000000000000000, 0.000000000000000000 ) ) ;
#7103 = DIRECTION ( 'NONE',  ( 0.000000000000000000, -1.530455820933490821E-32, 1.000000000000000000 ) ) ;
#7104 = DIRECTION ( 'NONE',  ( -1.000000000000000000, -1.031065855027150586E-29, 2.218671295934095703E-30 ) ) ;
#7105 = AXIS2_PLACEMENT_3D ( 'NONE', #6503, #1598, #12304 ) ;
#7106 = ORIENTED_EDGE ( 'NONE', *, *, #213, .T. ) ;
#7107 = CIRCLE ( 'NONE', #10602, 6.999999999999999112 ) ;
#7108 = DIRECTION ( 'NONE',  ( 1.000000000000000000, 1.081682119347366321E-16, -6.938893903907228378E-17 ) ) ;
#7109 = ADVANCED_FACE ( 'NONE', ( #12606 ), #12414, .T. ) ;
#7110 = CARTESIAN_POINT ( 'NONE',  ( 2.000000000000001776, 1.773042676681338303, 0.000000000000000000 ) ) ;
#7111 = CARTESIAN_POINT ( 'NONE',  ( -3.999999999999993339, 2.471528634177572847, -3.686887442155197370 ) ) ;
#7112 = FACE_OUTER_BOUND ( 'NONE', #6051, .T. ) ;
#7113 = ORIENTED_EDGE ( 'NONE', *, *, #12484, .T. ) ;
#7114 = DIRECTION ( 'NONE',  ( -1.000000000000000000, 1.010728034814421376E-30, 1.090846720500930387E-30 ) ) ;
#7115 = DIRECTION ( 'NONE',  ( 1.000000000000000000, 1.081682119347366197E-16, -6.938893903907228378E-17 ) ) ;
#7116 = PLANE ( 'NONE',  #8001 ) ;
#7117 = VECTOR ( 'NONE', #3940, 1000.000000000000000 ) ;
#7118 = ORIENTED_EDGE ( 'NONE', *, *, #2882, .F. ) ;
#7119 = CARTESIAN_POINT ( 'NONE',  ( 19.99999999999999645, 0.000000000000000000, 0.000000000000000000 ) ) ;
#7120 = ORIENTED_EDGE ( 'NONE', *, *, #5924, .F. ) ;
#7121 = ORIENTED_EDGE ( 'NONE', *, *, #2864, .F. ) ;
#7122 = SHAPE_DEFINITION_REPRESENTATION ( #8228, #2726 ) ;
#7123 = CARTESIAN_POINT ( 'NONE',  ( 14.00000000000000000, -13.00000000000000000, 6.000000000000001776 ) ) ;
#7124 = EDGE_LOOP ( 'NONE', ( #2299, #10420, #7182, #4208 ) ) ;
#7125 = DIRECTION ( 'NONE',  ( -1.000000000000000000, 0.000000000000000000, 0.000000000000000000 ) ) ;
#7126 = ADVANCED_FACE ( 'NONE', ( #10393 ), #9356, .T. ) ;
#7127 = FACE_OUTER_BOUND ( 'NONE', #10873, .T. ) ;
#7128 = EDGE_CURVE ( 'NONE', #3948, #10809, #1754, .T. ) ;
#7129 = ORIENTED_EDGE ( 'NONE', *, *, #6690, .T. ) ;
#7130 = DIRECTION ( 'NONE',  ( 0.000000000000000000, 0.000000000000000000, -1.000000000000000000 ) ) ;
#7131 = CARTESIAN_POINT ( 'NONE',  ( -3.999999999999994671, 0.000000000000000000, 8.673617379884035472E-15 ) ) ;
#7132 = CIRCLE ( 'NONE', #2836, 6.499000000000008548 ) ;
#7133 = DIRECTION ( 'NONE',  ( -3.437775699846489820E-17, -0.2951046417778627751, -0.9554649393887560960 ) ) ;
#7134 = CARTESIAN_POINT ( 'NONE',  ( -2.807080416178834525, 3.225969019225355616, -3.502507215260556528 ) ) ;
#7135 = EDGE_LOOP ( 'NONE', ( #11504, #8472, #11979, #773 ) ) ;
#7136 = VERTEX_POINT ( 'NONE', #6484 ) ;
#7137 = ORIENTED_EDGE ( 'NONE', *, *, #4838, .T. ) ;
#7138 = ORIENTED_EDGE ( 'NONE', *, *, #9318, .F. ) ;
#7139 = DIRECTION ( 'NONE',  ( 0.000000000000000000, 0.000000000000000000, 1.000000000000000000 ) ) ;
#7140 = CIRCLE ( 'NONE', #751, 4.000000000000000000 ) ;
#7141 = FACE_OUTER_BOUND ( 'NONE', #6811, .T. ) ;
#7142 = VERTEX_POINT ( 'NONE', #9545 ) ;
#7143 = EDGE_CURVE ( 'NONE', #11779, #12600, #11427, .T. ) ;
#7144 = CARTESIAN_POINT ( 'NONE',  ( 4.000000000000000000, 0.1981133338132478328, 8.576208590949790933E-18 ) ) ;
#7145 = ORIENTED_EDGE ( 'NONE', *, *, #1859, .F. ) ;
#7146 = ADVANCED_FACE ( 'NONE', ( #7506 ), #3528, .T. ) ;
#7147 = CYLINDRICAL_SURFACE ( 'NONE', #3184, 2.800000000000003819 ) ;
#7148 = ORIENTED_EDGE ( 'NONE', *, *, #10823, .F. ) ;
#7149 = ADVANCED_FACE ( 'NONE', ( #739 ), #1579, .T. ) ;
#7150 = AXIS2_PLACEMENT_3D ( 'NONE', #200, #1033, #3250 ) ;
#7151 = AXIS2_PLACEMENT_3D ( 'NONE', #10753, #3756, #9590 ) ;
#7152 = DIRECTION ( 'NONE',  ( -1.417484439069003486E-30, 0.9195277725514489076, 0.3930250316539278255 ) ) ;
#7153 = DIRECTION ( 'NONE',  ( 0.000000000000000000, 0.000000000000000000, -1.000000000000000000 ) ) ;
#7154 = ADVANCED_FACE ( 'NONE', ( #11629 ), #8466, .F. ) ;
#7155 = VERTEX_POINT ( 'NONE', #2824 ) ;
#7156 = LINE ( 'NONE', #2629, #11081 ) ;
#7157 = ORIENTED_EDGE ( 'NONE', *, *, #12716, .F. ) ;
#7158 = FACE_OUTER_BOUND ( 'NONE', #3530, .T. ) ;
#7159 = VECTOR ( 'NONE', #5968, 1000.000000000000000 ) ;
#7160 = DIRECTION ( 'NONE',  ( -6.938893903907224680E-17, 3.250006781153453386E-32, -1.000000000000000000 ) ) ;
#7161 = EDGE_CURVE ( 'NONE', #10498, #9362, #2763, .T. ) ;
#7162 = FACE_OUTER_BOUND ( 'NONE', #6584, .T. ) ;
#7163 = EDGE_CURVE ( 'NONE', #3101, #992, #6068, .T. ) ;
#7164 = CARTESIAN_POINT ( 'NONE',  ( -17.00000000000000000, -30.00000000000000000, 3.000000000000030198 ) ) ;
#7165 = CARTESIAN_POINT ( 'NONE',  ( 4.000000000000000000, -2.309401076758518911, -0.4999999999999917843 ) ) ;
#7166 = DIRECTION ( 'NONE',  ( -1.000000000000000000, 1.010728034814421376E-30, 1.090846720500930387E-30 ) ) ;
#7167 = CARTESIAN_POINT ( 'NONE',  ( 2.756197834950067982, 3.027510591568718823, -3.223146290109625944 ) ) ;
#7168 = DIRECTION ( 'NONE',  ( 0.000000000000000000, 0.000000000000000000, 1.000000000000000000 ) ) ;
#7169 = VERTEX_POINT ( 'NONE', #6984 ) ;
#7170 = DIRECTION ( 'NONE',  ( 0.000000000000000000, 0.5877852522924684742, 0.8090169943749507819 ) ) ;
#7171 = CARTESIAN_POINT ( 'NONE',  ( 0.000000000000000000, -6.459281472512953037, 1.243290685169352816 ) ) ;
#7172 = CIRCLE ( 'NONE', #1612, 2.499999999999998668 ) ;
#7173 = FACE_OUTER_BOUND ( 'NONE', #3151, .T. ) ;
#7174 = CARTESIAN_POINT ( 'NONE',  ( 19.99999999999997868, 6.544726022087254513, 0.6592800351837256878 ) ) ;
#7175 = VERTEX_POINT ( 'NONE', #8786 ) ;
#7176 = EDGE_CURVE ( 'NONE', #5244, #4187, #928, .T. ) ;
#7177 = CARTESIAN_POINT ( 'NONE',  ( 19.99999999999999645, 0.000000000000000000, 0.000000000000000000 ) ) ;
#7178 = CARTESIAN_POINT ( 'NONE',  ( 9.000000000000017764, -12.49999999999999112, -6.000000000000038192 ) ) ;
#7179 = ADVANCED_FACE ( 'NONE', ( #4076 ), #1894, .T. ) ;
#7180 = DIRECTION ( 'NONE',  ( 0.000000000000000000, 0.000000000000000000, 1.000000000000000000 ) ) ;
#7181 = AXIS2_PLACEMENT_3D ( 'NONE', #6742, #12479, #9741 ) ;
#7182 = ORIENTED_EDGE ( 'NONE', *, *, #12716, .T. ) ;
#7183 = DIRECTION ( 'NONE',  ( 1.140150527077241873E-30, 0.000000000000000000, -1.000000000000000000 ) ) ;
#7184 = ORIENTED_EDGE ( 'NONE', *, *, #12679, .F. ) ;
#7185 = VECTOR ( 'NONE', #5711, 1000.000000000000114 ) ;
#7186 = EDGE_LOOP ( 'NONE', ( #7630, #348, #886, #12201 ) ) ;
#7187 = ITEM_DEFINED_TRANSFORMATION ( 'NONE', 'NONE', #3658,  #12422 ) ;
#7188 = CARTESIAN_POINT ( 'NONE',  ( 20.00000000000000000, 0.000000000000000000, 0.000000000000000000 ) ) ;
#7189 = ORIENTED_EDGE ( 'NONE', *, *, #8131, .F. ) ;
#7190 = DIRECTION ( 'NONE',  ( -1.848892746611746419E-31, -1.000000000000000000, 3.250006781153460502E-32 ) ) ;
#7191 = DIRECTION ( 'NONE',  ( 0.000000000000000000, -1.000000000000000000, 0.000000000000000000 ) ) ;
#7192 = VECTOR ( 'NONE', #4063, 1000.000000000000000 ) ;
#7193 = CIRCLE ( 'NONE', #1629, 2.800000000000004263 ) ;
#7194 = CARTESIAN_POINT ( 'NONE',  ( 20.00000000000000000, 22.22477142302764008, -7.338293953734278396 ) ) ;
#7195 = VECTOR ( 'NONE', #6470, 1000.000000000000000 ) ;
#7196 = ADVANCED_FACE ( 'NONE', ( #6865 ), #11013, .F. ) ;
#7197 = CARTESIAN_POINT ( 'NONE',  ( -10.00000000000000178, 0.000000000000000000, 0.000000000000000000 ) ) ;
#7198 = ORIENTED_EDGE ( 'NONE', *, *, #65, .T. ) ;
#7199 = ORIENTED_EDGE ( 'NONE', *, *, #3969, .F. ) ;
#7200 = EDGE_CURVE ( 'NONE', #3169, #4417, #3809, .T. ) ;
#7201 = ORIENTED_EDGE ( 'NONE', *, *, #5800, .T. ) ;
#7202 = CIRCLE ( 'NONE', #195, 2.800000000000002931 ) ;
#7203 = EDGE_CURVE ( 'NONE', #5083, #9004, #11821, .T. ) ;
#7204 = EDGE_LOOP ( 'NONE', ( #6404, #3974, #2252, #4617 ) ) ;
#7205 = VECTOR ( 'NONE', #9644, 1000.000000000000000 ) ;
#7206 = CIRCLE ( 'NONE', #3322, 7.400000000000009237 ) ;
#7207 = DIRECTION ( 'NONE',  ( 0.000000000000000000, 1.000000000000000000, -1.467581828789149335E-15 ) ) ;
#7208 = EDGE_CURVE ( 'NONE', #12227, #10180, #12728, .T. ) ;
#7209 = PRODUCT ( 'hex flange nut gradea_iso_ISO - 4161 - M5 - N', 'hex flange nut gradea_iso_ISO - 4161 - M5 - N', '', ( #10976 ) ) ;
#7210 = CARTESIAN_POINT ( 'NONE',  ( 4.197310751797295403, 0.8178363989516003185, -3.502498386812445741 ) ) ;
#7211 = EDGE_LOOP ( 'NONE', ( #5275, #7406, #1521, #2766 ) ) ;
#7212 = DIRECTION ( 'NONE',  ( -1.000000000000000000, 1.010728034814421376E-30, 1.090846720500930387E-30 ) ) ;
#7213 = ORIENTED_EDGE ( 'NONE', *, *, #7611, .F. ) ;
#7214 = DIRECTION ( 'NONE',  ( 0.000000000000000000, 0.9909497617679351444, -0.1342332658176521587 ) ) ;
#7215 = DIRECTION ( 'NONE',  ( -1.387778780781445182E-16, 0.9997704357740726522, 0.02142605311579142552 ) ) ;
#7216 = CIRCLE ( 'NONE', #1028, 19.99999999999998934 ) ;
#7217 = AXIS2_PLACEMENT_3D ( 'NONE', #7090, #3243, #6116 ) ;
#7218 = CIRCLE ( 'NONE', #9253, 6.000000000000013323 ) ;
#7219 = DIRECTION ( 'NONE',  ( 0.000000000000000000, 1.530455820933490821E-32, -1.000000000000000000 ) ) ;
#7220 = CYLINDRICAL_SURFACE ( 'NONE', #5138, 6.499000000000010324 ) ;
#7221 = ORIENTED_EDGE ( 'NONE', *, *, #11619, .T. ) ;
#7222 = PLANE ( 'NONE',  #387 ) ;
#7223 = ORIENTED_EDGE ( 'NONE', *, *, #12732, .F. ) ;
#7224 = LINE ( 'NONE', #12117, #9903 ) ;
#7225 =( GEOMETRIC_REPRESENTATION_CONTEXT ( 3 ) GLOBAL_UNCERTAINTY_ASSIGNED_CONTEXT ( ( #9438 ) ) GLOBAL_UNIT_ASSIGNED_CONTEXT ( ( #4457, #1554, #9150 ) ) REPRESENTATION_CONTEXT ( 'NONE', 'WORKASPACE' ) );
#7226 = SURFACE_STYLE_USAGE ( .BOTH. , #3307 ) ;
#7227 = CARTESIAN_POINT ( 'NONE',  ( 19.99999999999997868, 5.280167904461786854, -3.922743398397314341 ) ) ;
#7228 = DIRECTION ( 'NONE',  ( -1.000000000000000000, 1.010728034814421376E-30, 1.090846720500930387E-30 ) ) ;
#7229 = EDGE_CURVE ( 'NONE', #12171, #5751, #7824, .T. ) ;
#7230 = EDGE_CURVE ( 'NONE', #962, #7688, #12380, .T. ) ;
#7231 = DIRECTION ( 'NONE',  ( -0.000000000000000000, 1.000000000000000000, -0.000000000000000000 ) ) ;
#7232 = CYLINDRICAL_SURFACE ( 'NONE', #12449, 4.000000000000000888 ) ;
#7233 = DIRECTION ( 'NONE',  ( 1.000000000000000000, 0.000000000000000000, 0.000000000000000000 ) ) ;
#7234 = VERTEX_POINT ( 'NONE', #8904 ) ;
#7235 = CARTESIAN_POINT ( 'NONE',  ( 19.99999999999997868, 5.956456411769428527, -2.790827096698922372 ) ) ;
#7236 = EDGE_CURVE ( 'NONE', #11879, #6259, #5054, .T. ) ;
#7237 = CARTESIAN_POINT ( 'NONE',  ( 14.00000000000000000, 30.00000000000000000, 0.000000000000000000 ) ) ;
#7238 = ADVANCED_FACE ( 'NONE', ( #90 ), #3955, .T. ) ;
#7239 = CIRCLE ( 'NONE', #5597, 4.000000000000008882 ) ;
#7240 = ORIENTED_EDGE ( 'NONE', *, *, #2280, .F. ) ;
#7241 = LINE ( 'NONE', #1173, #3159 ) ;
#7242 = ADVANCED_FACE ( 'NONE', ( #8844 ), #7878, .F. ) ;
#7243 = CARTESIAN_POINT ( 'NONE',  ( 19.99999999999997868, 6.359534927042317598, 1.339147681075194996 ) ) ;
#7244 = DIRECTION ( 'NONE',  ( 0.000000000000000000, 0.000000000000000000, 1.000000000000000000 ) ) ;
#7245 = DIRECTION ( 'NONE',  ( -0.000000000000000000, -1.000000000000000000, -0.000000000000000000 ) ) ;
#7246 = CARTESIAN_POINT ( 'NONE',  ( 4.200000000000001954, -1.221245327087672786E-16, -2.200000000000003730 ) ) ;
#7247 = AXIS2_PLACEMENT_3D ( 'NONE', #8181, #1222, #3116 ) ;
#7248 = DIRECTION ( 'NONE',  ( 1.000000000000000000, 0.000000000000000000, 0.000000000000000000 ) ) ;
#7249 = AXIS2_PLACEMENT_3D ( 'NONE', #853, #2874, #11681 ) ;
#7250 = ORIENTED_EDGE ( 'NONE', *, *, #8875, .F. ) ;
#7251 = CARTESIAN_POINT ( 'NONE',  ( 0.000000000000000000, 1.773042676681338303, 0.000000000000000000 ) ) ;
#7252 = ORIENTED_EDGE ( 'NONE', *, *, #10627, .F. ) ;
#7253 = EDGE_LOOP ( 'NONE', ( #10594, #1769, #8606, #7129 ) ) ;
#7254 = ORIENTED_EDGE ( 'NONE', *, *, #8694, .F. ) ;
#7255 = DIRECTION ( 'NONE',  ( -1.000000000000000000, 1.010728034814421376E-30, 1.090846720500930387E-30 ) ) ;
#7256 = EDGE_CURVE ( 'NONE', #9611, #7976, #30, .T. ) ;
#7257 = CARTESIAN_POINT ( 'NONE',  ( -17.00000000000000000, 2.632990618166788035E-16, 17.85000000000007248 ) ) ;
#7258 = VECTOR ( 'NONE', #10874, 1000.000000000000000 ) ;
#7259 = CYLINDRICAL_SURFACE ( 'NONE', #4450, 2.800000000000003819 ) ;
#7260 = DIRECTION ( 'NONE',  ( 0.000000000000000000, 0.000000000000000000, -1.000000000000000000 ) ) ;
#7261 = CARTESIAN_POINT ( 'NONE',  ( 2.000000000000001776, 0.000000000000000000, 0.000000000000000000 ) ) ;
#7262 = ORIENTED_EDGE ( 'NONE', *, *, #2270, .T. ) ;
#7263 = CARTESIAN_POINT ( 'NONE',  ( -3.522875095019470937, 2.820352903225139762, -3.598441714920489698 ) ) ;
#7264 = DIRECTION ( 'NONE',  ( 0.000000000000000000, 0.000000000000000000, -1.000000000000000000 ) ) ;
#7265 = VERTEX_POINT ( 'NONE', #9863 ) ;
#7266 = ORIENTED_EDGE ( 'NONE', *, *, #2811, .T. ) ;
#7267 = CIRCLE ( 'NONE', #9698, 2.800000000000004263 ) ;
#7268 = ORIENTED_EDGE ( 'NONE', *, *, #46, .T. ) ;
#7269 = AXIS2_PLACEMENT_3D ( 'NONE', #12627, #2786, #5656 ) ;
#7270 = EDGE_LOOP ( 'NONE', ( #4009, #3018 ) ) ;
#7271 = PLANE ( 'NONE',  #8484 ) ;
#7272 = VERTEX_POINT ( 'NONE', #3135 ) ;
#7273 = CARTESIAN_POINT ( 'NONE',  ( 27.00000000000001421, 40.41548023366553366, -10.14535464186970870 ) ) ;
#7274 = EDGE_LOOP ( 'NONE', ( #1922, #9378, #6431, #3074 ) ) ;
#7275 = CIRCLE ( 'NONE', #4177, 2.499999999999998668 ) ;
#7276 = CARTESIAN_POINT ( 'NONE',  ( -2.804994570502143070, -3.229033611042466223, -3.526374918436845807 ) ) ;
#7277 = EDGE_CURVE ( 'NONE', #3589, #7374, #3429, .T. ) ;
#7278 = CARTESIAN_POINT ( 'NONE',  ( 14.00000000000000000, -30.00000000000000000, 0.000000000000000000 ) ) ;
#7279 = EDGE_CURVE ( 'NONE', #3906, #10905, #11434, .T. ) ;
#7280 = CARTESIAN_POINT ( 'NONE',  ( 0.000000000000000000, 7.380072687735796499, -0.5427035320837090282 ) ) ;
#7281 = CARTESIAN_POINT ( 'NONE',  ( 19.99999999999999645, 1.052479792859053020, 6.413211932068313637 ) ) ;
#7282 = ORIENTED_EDGE ( 'NONE', *, *, #7748, .F. ) ;
#7283 = EDGE_LOOP ( 'NONE', ( #12294, #10776, #9997, #3420 ) ) ;
#7284 = CARTESIAN_POINT ( 'NONE',  ( 0.1999999999999987899, 0.000000000000000000, 3.299999999999982503 ) ) ;
#7285 = FILL_AREA_STYLE_COLOUR ( '', #2079 ) ;
#7286 = DIRECTION ( 'NONE',  ( -0.000000000000000000, 1.000000000000000000, 0.000000000000000000 ) ) ;
#7287 = CARTESIAN_POINT ( 'NONE',  ( 0.000000000000000000, 0.000000000000000000, 0.000000000000000000 ) ) ;
#7288 = EDGE_CURVE ( 'NONE', #9393, #3905, #8967, .T. ) ;
#7289 = AXIS2_PLACEMENT_3D ( 'NONE', #3693, #718, #7969 ) ;
#7290 = PRODUCT_DEFINITION ( 'UNKNOWN', '', #5288, #7087 ) ;
#7291 = DIRECTION ( 'NONE',  ( -1.000000000000000000, 1.010728034814421376E-30, 1.090846720500930387E-30 ) ) ;
#7292 = DIRECTION ( 'NONE',  ( 0.000000000000000000, 0.000000000000000000, 1.000000000000000000 ) ) ;
#7293 = CYLINDRICAL_SURFACE ( 'NONE', #7798, 2.800000000000003819 ) ;
#7294 = ORIENTED_EDGE ( 'NONE', *, *, #9146, .T. ) ;
#7295 = DIRECTION ( 'NONE',  ( 0.000000000000000000, -0.5128992774058948045, -0.8584487936018728726 ) ) ;
#7296 = CIRCLE ( 'NONE', #9733, 4.000000000000000000 ) ;
#7297 = CARTESIAN_POINT ( 'NONE',  ( 19.99999999999999645, -6.577476285968334224, -0.06996125000500313940 ) ) ;
#7298 = EDGE_LOOP ( 'NONE', ( #3348, #10484, #5028, #1329 ) ) ;
#7299 = ADVANCED_FACE ( 'NONE', ( #152 ), #7734, .T. ) ;
#7300 = CARTESIAN_POINT ( 'NONE',  ( -4.211140560182210280, 2.431303136016527144, -3.745885042887430405 ) ) ;
#7301 = DIRECTION ( 'NONE',  ( 0.000000000000000000, 0.000000000000000000, 1.000000000000000000 ) ) ;
#7303 = CARTESIAN_POINT ( 'NONE',  ( -3.999999999999993339, 0.8730739991738295513, -3.223134629628441328 ) ) ;
#7302 = VECTOR ( 'NONE', #7418, 1000.000000000000000 ) ;
#7304 = ADVANCED_FACE ( 'NONE', ( #12667 ), #9095, .T. ) ;
#7305 = LINE ( 'NONE', #11290, #6111 ) ;
#7306 = AXIS2_PLACEMENT_3D ( 'NONE', #6237, #374, #10883 ) ;
#7307 = FACE_OUTER_BOUND ( 'NONE', #3653, .T. ) ;
#7308 = EDGE_CURVE ( 'NONE', #2771, #9874, #1762, .T. ) ;
#7309 = AXIS2_PLACEMENT_3D ( 'NONE', #516, #12382, #4382 ) ;
#7310 = DIRECTION ( 'NONE',  ( 0.000000000000000000, -1.530455820933490821E-32, 1.000000000000000000 ) ) ;
#7311 = ORIENTED_EDGE ( 'NONE', *, *, #1595, .T. ) ;
#7312 = EDGE_CURVE ( 'NONE', #6675, #9760, #8195, .T. ) ;
#7313 = CARTESIAN_POINT ( 'NONE',  ( 19.99999999999997868, 7.100173756228414845, 2.085073771204572157 ) ) ;
#7314 = ORIENTED_EDGE ( 'NONE', *, *, #8711, .F. ) ;
#7315 = AXIS2_PLACEMENT_3D ( 'NONE', #12432, #12240, #2579 ) ;
#7316 = ORIENTED_EDGE ( 'NONE', *, *, #2550, .T. ) ;
#7317 = ITEM_DEFINED_TRANSFORMATION ( 'NONE', 'NONE', #6310,  #12422 ) ;
#7318 = CIRCLE ( 'NONE', #12048, 6.499000000000009436 ) ;
#7319 = VERTEX_POINT ( 'NONE', #6265 ) ;
#7320 = DIRECTION ( 'NONE',  ( -1.000000000000000000, 0.000000000000000000, 1.301042606982605074E-16 ) ) ;
#7321 = DIRECTION ( 'NONE',  ( -0.7071067811865348052, 3.925231146708775397E-17, 0.7071067811865602293 ) ) ;
#7322 = DIRECTION ( 'NONE',  ( 0.000000000000000000, 5.551115123125776539E-17, 1.000000000000000000 ) ) ;
#7323 = DIRECTION ( 'NONE',  ( -3.260214209858708648E-30, -0.5000000000000012212, -0.8660254037844380415 ) ) ;
#7324 = ORIENTED_EDGE ( 'NONE', *, *, #3180, .F. ) ;
#7325 = LINE ( 'NONE', #614, #1138 ) ;
#7326 = AXIS2_PLACEMENT_3D ( 'NONE', #7177, #5114, #2351 ) ;
#7327 = CARTESIAN_POINT ( 'NONE',  ( 19.99999999999999645, 3.019282868015074506, 6.756029230465976809 ) ) ;
#7328 = ORIENTED_EDGE ( 'NONE', *, *, #2349, .F. ) ;
#7329 = EDGE_LOOP ( 'NONE', ( #2572, #1155, #3776, #3537 ) ) ;
#7330 = ORIENTED_EDGE ( 'NONE', *, *, #10773, .F. ) ;
#7331 = VERTEX_POINT ( 'NONE', #9156 ) ;
#7332 = DIRECTION ( 'NONE',  ( 1.140150527077241873E-30, 0.000000000000000000, -1.000000000000000000 ) ) ;
#7333 = DIRECTION ( 'NONE',  ( -1.000000000000000000, -1.081682119347366444E-16, 6.938893903907229610E-17 ) ) ;
#7334 = ORIENTED_EDGE ( 'NONE', *, *, #2616, .F. ) ;
#7335 = VECTOR ( 'NONE', #4107, 1000.000000000000000 ) ;
#7336 = CARTESIAN_POINT ( 'NONE',  ( 0.000000000000000000, 1.834336845376708602, 6.234758161925244124 ) ) ;
#7337 = ORIENTED_EDGE ( 'NONE', *, *, #6247, .T. ) ;
#7338 = DIRECTION ( 'NONE',  ( 0.000000000000000000, 0.5128992774059070170, -0.8584487936018656562 ) ) ;
#7339 = LINE ( 'NONE', #2069, #5651 ) ;
#7340 = ADVANCED_FACE ( 'NONE', ( #6075, #7307 ), #9281, .F. ) ;
#7341 = CARTESIAN_POINT ( 'NONE',  ( 40.00000000000000711, 8.901672616175323682, -15.56445005073997478 ) ) ;
#7342 = AXIS2_PLACEMENT_3D ( 'NONE', #4550, #10256, #11247 ) ;
#7343 = CARTESIAN_POINT ( 'NONE',  ( 19.99999999999999645, 0.000000000000000000, 0.000000000000000000 ) ) ;
#7344 = STYLED_ITEM ( 'NONE', ( #4481 ), #5956 ) ;
#7345 = EDGE_LOOP ( 'NONE', ( #9744, #9259, #2795, #3398 ) ) ;
#7346 = ORIENTED_EDGE ( 'NONE', *, *, #5952, .T. ) ;
#7347 = DIRECTION ( 'NONE',  ( 0.000000000000000000, 0.000000000000000000, 1.000000000000000000 ) ) ;
#7348 = CARTESIAN_POINT ( 'NONE',  ( 0.000000000000000000, -0.8865213383406691516, 1.535500000000002085 ) ) ;
#7349 = AXIS2_PLACEMENT_3D ( 'NONE', #1796, #763, #6640 ) ;
#7350 = AXIS2_PLACEMENT_3D ( 'NONE', #5112, #8126, #2218 ) ;
#7351 = CARTESIAN_POINT ( 'NONE',  ( 11.17157287525379772, 12.99999999999999822, -2.828427124746177856 ) ) ;
#7352 = AXIS2_PLACEMENT_3D ( 'NONE', #846, #2992, #3938 ) ;
#7353 = CARTESIAN_POINT ( 'NONE',  ( 9.285714285714284699, -3.469446951953614189E-15, -3.711537444790451001 ) ) ;
#7354 = DIRECTION ( 'NONE',  ( 1.140150527077241873E-30, 0.000000000000000000, -1.000000000000000000 ) ) ;
#7355 = PLANE ( 'NONE',  #6776 ) ;
#7356 = ORIENTED_EDGE ( 'NONE', *, *, #5832, .F. ) ;
#7357 = DIRECTION ( 'NONE',  ( 1.140150527077241873E-30, 0.000000000000000000, -1.000000000000000000 ) ) ;
#7358 = B_SPLINE_CURVE_WITH_KNOTS ( 'NONE', 3,
 ( #9324, #5541, #4447, #3490, #1543, #5477 ),
 .UNSPECIFIED., .F., .F.,
 ( 4, 2, 4 ),
 ( 0.002365888236227973833, 0.003551327329835075874, 0.004736766423442177916 ),
 .UNSPECIFIED. ) ;
#7359 = AXIS2_PLACEMENT_3D ( 'NONE', #3088, #12096, #5132 ) ;
#7360 = CARTESIAN_POINT ( 'NONE',  ( 0.000000000000000000, 5.012092988314003073, -4.137139697483478429 ) ) ;
#7361 = EDGE_CURVE ( 'NONE', #5977, #1661, #12672, .T. ) ;
#7362 = EDGE_CURVE ( 'NONE', #1057, #8600, #5058, .T. ) ;
#7363 = EDGE_CURVE ( 'NONE', #10248, #4329, #1147, .T. ) ;
#7364 = ORIENTED_EDGE ( 'NONE', *, *, #2345, .T. ) ;
#7365 = LINE ( 'NONE', #3691, #60 ) ;
#7366 = FACE_OUTER_BOUND ( 'NONE', #6802, .T. ) ;
#7367 = DIRECTION ( 'NONE',  ( -1.000000000000000000, 1.010728034814421376E-30, 1.090846720500930387E-30 ) ) ;
#7368 = DIRECTION ( 'NONE',  ( 5.115269932292490543E-31, -0.9195277725514543476, 0.3930250316539146693 ) ) ;
#7369 = CYLINDRICAL_SURFACE ( 'NONE', #5664, 6.000000000000000000 ) ;
#7370 = CARTESIAN_POINT ( 'NONE',  ( 0.000000000000000000, 3.565124043461764813, -5.527927226701604191 ) ) ;
#7371 = SURFACE_STYLE_FILL_AREA ( #10239 ) ;
#7372 = ORIENTED_EDGE ( 'NONE', *, *, #3258, .F. ) ;
#7373 = CARTESIAN_POINT ( 'NONE',  ( -31.74999999999995026, 0.000000000000000000, -1.734723475976807094E-14 ) ) ;
#7374 = VERTEX_POINT ( 'NONE', #11034 ) ;
#7375 = ORIENTED_EDGE ( 'NONE', *, *, #6267, .F. ) ;
#7376 = ORIENTED_EDGE ( 'NONE', *, *, #12431, .F. ) ;
#7377 = VERTEX_POINT ( 'NONE', #3202 ) ;
#7378 = FACE_OUTER_BOUND ( 'NONE', #9057, .T. ) ;
#7379 = CARTESIAN_POINT ( 'NONE',  ( 0.000000000000000000, 0.000000000000000000, 0.000000000000000000 ) ) ;
#7380 = CARTESIAN_POINT ( 'NONE',  ( 12.94787914004603202, 30.00000000000000000, 5.638155724715463890 ) ) ;
#7381 = CARTESIAN_POINT ( 'NONE',  ( 15.00000000000003375, 30.00000000000001776, -9.742497179615118866E-31 ) ) ;
#7382 = EDGE_LOOP ( 'NONE', ( #5446, #730 ) ) ;
#7383 = EDGE_CURVE ( 'NONE', #8798, #7604, #4228, .T. ) ;
#7384 = CARTESIAN_POINT ( 'NONE',  ( 2.000000000000001776, 1.028071432934799421E-16, -1.535500000000001863 ) ) ;
#7385 = VECTOR ( 'NONE', #10404, 1000.000000000000000 ) ;
#7386 = CARTESIAN_POINT ( 'NONE',  ( 0.000000000000000000, -7.399010254356644722, 0.1210258481698957278 ) ) ;
#7387 = VERTEX_POINT ( 'NONE', #1180 ) ;
#7388 = VERTEX_POINT ( 'NONE', #4401 ) ;
#7389 = ORIENTED_EDGE ( 'NONE', *, *, #10112, .F. ) ;
#7390 = ORIENTED_EDGE ( 'NONE', *, *, #2751, .F. ) ;
#7391 = EDGE_CURVE ( 'NONE', #1191, #2734, #10175, .T. ) ;
#7392 = DIRECTION ( 'NONE',  ( 0.000000000000000000, 0.000000000000000000, 1.000000000000000000 ) ) ;
#7393 = ADVANCED_FACE ( 'NONE', ( #8129 ), #3266, .T. ) ;
#7394 = CIRCLE ( 'NONE', #5737, 6.499000000000009436 ) ;
#7395 = LINE ( 'NONE', #2442, #12692 ) ;
#7396 = EDGE_LOOP ( 'NONE', ( #8835, #6649, #7812, #807 ) ) ;
#7397 = CARTESIAN_POINT ( 'NONE',  ( 9.999999999999980460, -3.612733913993546597, -6.458185013351741333 ) ) ;
#7398 = VECTOR ( 'NONE', #3024, 1000.000000000000000 ) ;
#7399 = ORIENTED_EDGE ( 'NONE', *, *, #8671, .F. ) ;
#7400 = CARTESIAN_POINT ( 'NONE',  ( 9.999999999999998224, 6.057062246029580876, -4.251117141143418543 ) ) ;
#7401 = LINE ( 'NONE', #11332, #7499 ) ;
#7402 = CARTESIAN_POINT ( 'NONE',  ( 0.000000000000000000, 0.000000000000000000, 0.000000000000000000 ) ) ;
#7403 = AXIS2_PLACEMENT_3D ( 'NONE', #4897, #3929, #9641 ) ;
#7404 = AXIS2_PLACEMENT_3D ( 'NONE', #3968, #9041, #9934 ) ;
#7405 = DIRECTION ( 'NONE',  ( -1.000000000000000000, -2.206481006425900381E-16, 8.674603474570138454E-17 ) ) ;
#7406 = ORIENTED_EDGE ( 'NONE', *, *, #7518, .F. ) ;
#7407 = AXIS2_PLACEMENT_3D ( 'NONE', #9411, #609, #5444 ) ;
#7408 = EDGE_LOOP ( 'NONE', ( #5775, #2899, #9242, #9935, #4425, #12625, #1899, #2504 ) ) ;
#7409 = CARTESIAN_POINT ( 'NONE',  ( 9.999999999999998224, 7.358375340956999189, 0.7837807994561865055 ) ) ;
#7410 =( LENGTH_UNIT ( ) NAMED_UNIT ( * ) SI_UNIT ( .MILLI., .METRE. ) );
#7411 = DIRECTION ( 'NONE',  ( 0.000000000000000000, 0.000000000000000000, 1.000000000000000000 ) ) ;
#7412 = VECTOR ( 'NONE', #12354, 1000.000000000000000 ) ;
#7413 = CIRCLE ( 'NONE', #7609, 2.800000000000002931 ) ;
#7414 = AXIS2_PLACEMENT_3D ( 'NONE', #2865, #7860, #3051 ) ;
#7415 = DIRECTION ( 'NONE',  ( -1.000000000000000000, 1.010728034814421376E-30, 1.090846720500930387E-30 ) ) ;
#7416 = ADVANCED_FACE ( 'NONE', ( #3450 ), #11100, .T. ) ;
#7417 = DIRECTION ( 'NONE',  ( 0.000000000000000000, 1.000000000000000000, 0.000000000000000000 ) ) ;
#7418 = DIRECTION ( 'NONE',  ( -1.000000000000000000, 1.010728034814421376E-30, 1.090846720500930387E-30 ) ) ;
#7419 = FACE_OUTER_BOUND ( 'NONE', #12406, .T. ) ;
#7420 = VERTEX_POINT ( 'NONE', #1366 ) ;
#7422 = CARTESIAN_POINT ( 'NONE',  ( 0.6666666666666680729, 4.233901974057235229, -3.300726591567098023 ) ) ;
#7421 = PRESENTATION_LAYER_ASSIGNMENT (  '', '', ( #12372 ) ) ;
#7423 = LINE ( 'NONE', #10298, #11573 ) ;
#7424 = PRESENTATION_STYLE_ASSIGNMENT (( #12259 ) ) ;
#7425 = CARTESIAN_POINT ( 'NONE',  ( 0.000000000000000000, 0.3649881613860921359, -6.567714405409697420 ) ) ;
#7426 = ORIENTED_EDGE ( 'NONE', *, *, #10353, .F. ) ;
#7427 = CARTESIAN_POINT ( 'NONE',  ( 14.00000000000000000, 13.00000000000000000, 6.000000000000001776 ) ) ;
#7428 = DIRECTION ( 'NONE',  ( 0.000000000000000000, 0.000000000000000000, 1.000000000000000000 ) ) ;
#7429 = CARTESIAN_POINT ( 'NONE',  ( -10.00000000000000178, 0.000000000000000000, 0.000000000000000000 ) ) ;
#7430 = CYLINDRICAL_SURFACE ( 'NONE', #11035, 10.00000000000000000 ) ;
#7431 = EDGE_CURVE ( 'NONE', #8682, #6675, #7107, .T. ) ;
#7432 = DIRECTION ( 'NONE',  ( 0.000000000000000000, 1.000000000000000000, 0.000000000000000000 ) ) ;
#7433 = EDGE_CURVE ( 'NONE', #6622, #4036, #530, .T. ) ;
#7434 = DIRECTION ( 'NONE',  ( -1.000000000000000000, 0.000000000000000000, 0.000000000000000000 ) ) ;
#7435 = PRESENTATION_STYLE_ASSIGNMENT (( #9345 ) ) ;
#7436 = ORIENTED_EDGE ( 'NONE', *, *, #4435, .F. ) ;
#7437 = VECTOR ( 'NONE', #9723, 1000.000000000000000 ) ;
#7438 = CONTEXT_DEPENDENT_SHAPE_REPRESENTATION ( #2652, #8727 ) ;
#7439 = ORIENTED_EDGE ( 'NONE', *, *, #7383, .F. ) ;
#7440 = ORIENTED_EDGE ( 'NONE', *, *, #9484, .F. ) ;
#7441 = DIRECTION ( 'NONE',  ( 1.000000000000000000, -1.010728034814421376E-30, -1.090846720500930387E-30 ) ) ;
#7442 = DIRECTION ( 'NONE',  ( -1.000000000000000000, 1.010728034814421376E-30, 1.090846720500930387E-30 ) ) ;
#7443 = CARTESIAN_POINT ( 'NONE',  ( 14.00000000000000000, 30.00000000000000000, 0.000000000000000000 ) ) ;
#7444 = AXIS2_PLACEMENT_3D ( 'NONE', #451, #1606, #9513 ) ;
#7445 = FACE_OUTER_BOUND ( 'NONE', #9112, .T. ) ;
#7446 = ORIENTED_EDGE ( 'NONE', *, *, #8690, .T. ) ;
#7447 = DIRECTION ( 'NONE',  ( 0.000000000000000000, 0.000000000000000000, 1.000000000000000000 ) ) ;
#7448 = EDGE_CURVE ( 'NONE', #8530, #1584, #6708, .T. ) ;
#7449 = CYLINDRICAL_SURFACE ( 'NONE', #6597, 7.400000000000010125 ) ;
#7450 = ORIENTED_EDGE ( 'NONE', *, *, #8120, .F. ) ;
#7451 = VERTEX_POINT ( 'NONE', #12208 ) ;
#7452 = DIRECTION ( 'NONE',  ( 0.000000000000000000, 0.000000000000000000, 1.000000000000000000 ) ) ;
#7453 = VERTEX_POINT ( 'NONE', #10235 ) ;
#7454 = VERTEX_POINT ( 'NONE', #2415 ) ;
#7455 = AXIS2_PLACEMENT_3D ( 'NONE', #3368, #11208, #3430 ) ;
#7456 = ORIENTED_EDGE ( 'NONE', *, *, #5447, .F. ) ;
#7457 = CARTESIAN_POINT ( 'NONE',  ( -17.00000000000002842, 19.99999999999998579, 14.15000000000003588 ) ) ;
#7458 = DIRECTION ( 'NONE',  ( 0.000000000000000000, -0.5000000000000012212, -0.8660254037844380415 ) ) ;
#7459 = ORIENTED_EDGE ( 'NONE', *, *, #7700, .T. ) ;
#7460 = CARTESIAN_POINT ( 'NONE',  ( 2.000000000000001776, 1.329782007511000286, 0.7677500000000045954 ) ) ;
#7461 = CARTESIAN_POINT ( 'NONE',  ( 0.000000000000000000, 0.000000000000000000, 0.000000000000000000 ) ) ;
#7462 = EDGE_CURVE ( 'NONE', #9064, #2371, #5871, .T. ) ;
#7463 = VECTOR ( 'NONE', #7108, 1000.000000000000000 ) ;
#7464 = DIRECTION ( 'NONE',  ( 0.000000000000000000, -0.08963930890344089242, 0.9959742939952382912 ) ) ;
#7465 = CONICAL_SURFACE ( 'NONE', #3564, 2.500000000000000888, 0.9599310885968785900 ) ;
#7466 = EDGE_CURVE ( 'NONE', #11564, #2762, #11645, .T. ) ;
#7467 = CARTESIAN_POINT ( 'NONE',  ( 0.000000000000000000, 0.000000000000000000, -0.2800830152838839626 ) ) ;
#7468 = EDGE_LOOP ( 'NONE', ( #8269, #5582 ) ) ;
#7469 = VERTEX_POINT ( 'NONE', #8581 ) ;
#7470 = DIRECTION ( 'NONE',  ( 0.000000000000000000, 0.000000000000000000, 1.000000000000000000 ) ) ;
#7471 = ADVANCED_FACE ( 'NONE', ( #1625 ), #5497, .F. ) ;
#7472 = VECTOR ( 'NONE', #9749, 1000.000000000000000 ) ;
#7473 = DIRECTION ( 'NONE',  ( 0.000000000000000000, 0.000000000000000000, 1.000000000000000000 ) ) ;
#7474 = CYLINDRICAL_SURFACE ( 'NONE', #388, 7.400000000000010125 ) ;
#7475 = DIRECTION ( 'NONE',  ( -2.218671295934093601E-30, 5.551115123125776539E-17, 1.000000000000000000 ) ) ;
#7476 = CARTESIAN_POINT ( 'NONE',  ( 0.000000000000000000, -2.099089055167822071, 6.233932467347762518 ) ) ;
#7477 = CIRCLE ( 'NONE', #7699, 6.499000000000011212 ) ;
#7478 = CARTESIAN_POINT ( 'NONE',  ( 11.17157287525379772, 30.00000000000000000, -2.828427124746177856 ) ) ;
#7479 = VERTEX_POINT ( 'NONE', #5618 ) ;
#7480 = CARTESIAN_POINT ( 'NONE',  ( 19.99999999999999645, -6.486618105788070743, -0.4009819817180210189 ) ) ;
#7481 = FACE_OUTER_BOUND ( 'NONE', #5793, .T. ) ;
#7482 = DIRECTION ( 'NONE',  ( 0.000000000000000000, 0.7818314824680310249, -0.6234898018587319291 ) ) ;
#7483 = CIRCLE ( 'NONE', #7289, 2.499999999999999556 ) ;
#7484 = VERTEX_POINT ( 'NONE', #9530 ) ;
#7485 = APPLICATION_CONTEXT ( 'automotive_design' ) ;
#7486 = DIRECTION ( 'NONE',  ( -1.000000000000000000, 1.010728034814421376E-30, 1.090846720500930387E-30 ) ) ;
#7487 = LINE ( 'NONE', #11161, #6880 ) ;
#7488 = DIRECTION ( 'NONE',  ( -1.000000000000000000, 1.010728034814421376E-30, 1.090846720500930387E-30 ) ) ;
#7489 = CARTESIAN_POINT ( 'NONE',  ( 0.000000000000000000, -0.8865213383406727043, 1.535500000000009191 ) ) ;
#7490 = DIRECTION ( 'NONE',  ( -1.000000000000000000, 0.000000000000000000, 0.000000000000000000 ) ) ;
#7491 = CIRCLE ( 'NONE', #7894, 6.499000000000008548 ) ;
#7492 = LINE ( 'NONE', #12401, #10356 ) ;
#7493 = DIRECTION ( 'NONE',  ( 0.000000000000000000, 1.000000000000000000, 0.000000000000000000 ) ) ;
#7494 = DIRECTION ( 'NONE',  ( 5.115269932292492295E-31, -0.9195277725514543476, 0.3930250316539147248 ) ) ;
#7495 = EDGE_LOOP ( 'NONE', ( #8409, #12176, #9305, #2613 ) ) ;
#7496 = ADVANCED_FACE ( 'NONE', ( #4720 ), #1563, .T. ) ;
#7497 = AXIS2_PLACEMENT_3D ( 'NONE', #7924, #4974, #8713 ) ;
#7498 = ORIENTED_EDGE ( 'NONE', *, *, #2954, .T. ) ;
#7499 = VECTOR ( 'NONE', #1531, 1000.000000000000000 ) ;
#7500 = VERTEX_POINT ( 'NONE', #8389 ) ;
#7501 = FACE_OUTER_BOUND ( 'NONE', #10181, .T. ) ;
#7502 = FILL_AREA_STYLE_COLOUR ( '', #5891 ) ;
#7503 = DIRECTION ( 'NONE',  ( 0.000000000000000000, 0.6579387259397136978, -0.7530714660036098573 ) ) ;
#7504 = DIRECTION ( 'NONE',  ( -7.025792437124625182E-30, -0.4999999999999992784, 0.8660254037844390407 ) ) ;
#7505 = VERTEX_POINT ( 'NONE', #2478 ) ;
#7506 = FACE_OUTER_BOUND ( 'NONE', #10458, .T. ) ;
#7507 = CARTESIAN_POINT ( 'NONE',  ( -11.83215956619923226, 30.00000000000000000, 1.999999999999999556 ) ) ;
#7508 = ORIENTED_EDGE ( 'NONE', *, *, #6225, .T. ) ;
#7509 = CIRCLE ( 'NONE', #1946, 2.500000000000003553 ) ;
#7510 = AXIS2_PLACEMENT_3D ( 'NONE', #3011, #863, #5946 ) ;
#7511 = ORIENTED_EDGE ( 'NONE', *, *, #3692, .F. ) ;
#7512 = DIRECTION ( 'NONE',  ( 1.154721252774410375E-34, -3.250006781153453386E-32, 1.000000000000000000 ) ) ;
#7513 = ORIENTED_EDGE ( 'NONE', *, *, #1145, .F. ) ;
#7514 = VERTEX_POINT ( 'NONE', #2677 ) ;
#7515 = FILL_AREA_STYLE_COLOUR ( '', #2284 ) ;
#7516 = ADVANCED_FACE ( 'NONE', ( #12521 ), #2546, .T. ) ;
#7517 = EDGE_CURVE ( 'NONE', #35, #11636, #9400, .T. ) ;
#7518 = EDGE_CURVE ( 'NONE', #5416, #701, #11291, .T. ) ;
#7519 = ORIENTED_EDGE ( 'NONE', *, *, #1914, .F. ) ;
#7520 = CARTESIAN_POINT ( 'NONE',  ( 20.00000000000000355, 40.41548023366552655, -10.14535464186970515 ) ) ;
#7521 = CARTESIAN_POINT ( 'NONE',  ( 19.99999999999999645, 0.000000000000000000, 0.000000000000000000 ) ) ;
#7522 = ORIENTED_EDGE ( 'NONE', *, *, #4759, .T. ) ;
#7523 = CARTESIAN_POINT ( 'NONE',  ( 2.000000000000007105, -3.464101615137750390, -1.734723475976807094E-14 ) ) ;
#7524 = DIRECTION ( 'NONE',  ( 0.000000000000000000, -5.551115123125770376E-17, -1.000000000000000000 ) ) ;
#7525 = CARTESIAN_POINT ( 'NONE',  ( 0.000000000000000000, 0.000000000000000000, 0.000000000000000000 ) ) ;
#7526 = DIRECTION ( 'NONE',  ( -0.5000000000000056621, 4.807406715958370281E-17, 0.8660254037844352659 ) ) ;
#7527 = ORIENTED_EDGE ( 'NONE', *, *, #10033, .T. ) ;
#7528 = ORIENTED_EDGE ( 'NONE', *, *, #7713, .F. ) ;
#7529 = FACE_OUTER_BOUND ( 'NONE', #3110, .T. ) ;
#7530 = VECTOR ( 'NONE', #9246, 1000.000000000000000 ) ;
#7531 = DIRECTION ( 'NONE',  ( -1.000000000000000000, -2.891205793294682271E-16, 8.326672684688674053E-17 ) ) ;
#7532 = ORIENTED_EDGE ( 'NONE', *, *, #10892, .T. ) ;
#7533 = CARTESIAN_POINT ( 'NONE',  ( 19.99999999999999645, 5.895746314278407674, 2.916892913127008935 ) ) ;
#7534 = DIRECTION ( 'NONE',  ( 0.000000000000000000, 0.000000000000000000, 1.000000000000000000 ) ) ;
#7535 = AXIS2_PLACEMENT_3D ( 'NONE', #1704, #9543, #12222 ) ;
#7536 = ADVANCED_FACE ( 'NONE', ( #536 ), #7369, .T. ) ;
#7537 = CIRCLE ( 'NONE', #9171, 7.400000000000011902 ) ;
#7538 = LINE ( 'NONE', #9327, #502 ) ;
#7539 = CARTESIAN_POINT ( 'NONE',  ( 19.99999999999997868, 5.362412286431509578, -3.809543717993867595 ) ) ;
#7540 = ORIENTED_EDGE ( 'NONE', *, *, #804, .F. ) ;
#7541 = DIRECTION ( 'NONE',  ( -1.000000000000000000, 1.010728034814421376E-30, 1.090846720500930387E-30 ) ) ;
#7542 = CARTESIAN_POINT ( 'NONE',  ( 40.00000000000000711, 18.52447679111068268, -16.77732469694377926 ) ) ;
#7543 = AXIS2_PLACEMENT_3D ( 'NONE', #8262, #1813, #781 ) ;
#7544 = EDGE_CURVE ( 'NONE', #1466, #8041, #7551, .T. ) ;
#7545 = EDGE_CURVE ( 'NONE', #6728, #4892, #3624, .T. ) ;
#7546 = FACE_OUTER_BOUND ( 'NONE', #4559, .T. ) ;
#7547 = CARTESIAN_POINT ( 'NONE',  ( 19.99999999999997868, -7.258495115966583811, 1.440225208600806717 ) ) ;
#7548 = CYLINDRICAL_SURFACE ( 'NONE', #81, 7.400000000000010125 ) ;
#7549 = LINE ( 'NONE', #11555, #4047 ) ;
#7550 = DIRECTION ( 'NONE',  ( -1.000000000000000000, 1.010728034814421376E-30, 1.090846720500930387E-30 ) ) ;
#7551 = LINE ( 'NONE', #11557, #9357 ) ;
#7552 = AXIS2_PLACEMENT_3D ( 'NONE', #6308, #11406, #12567 ) ;
#7553 = AXIS2_PLACEMENT_3D ( 'NONE', #11866, #3117, #4060 ) ;
#7554 = DIRECTION ( 'NONE',  ( -0.000000000000000000, -0.000000000000000000, -1.000000000000000000 ) ) ;
#7555 = AXIS2_PLACEMENT_3D ( 'NONE', #5904, #4757, #3975 ) ;
#7556 = CYLINDRICAL_SURFACE ( 'NONE', #11519, 7.400000000000010125 ) ;
#7557 = DIRECTION ( 'NONE',  ( 0.000000000000000000, 0.9554649393887557629, -0.2951046417778634412 ) ) ;
#7558 = ORIENTED_EDGE ( 'NONE', *, *, #4468, .F. ) ;
#7559 = ORIENTED_EDGE ( 'NONE', *, *, #6753, .T. ) ;
#7560 = ORIENTED_EDGE ( 'NONE', *, *, #4351, .T. ) ;
#7561 = EDGE_CURVE ( 'NONE', #1901, #10923, #3697, .T. ) ;
#7562 = CARTESIAN_POINT ( 'NONE',  ( -2.099999999999965450, -3.212271124132670141E-15, -4.694516984716123886 ) ) ;
#7563 = DIRECTION ( 'NONE',  ( -1.000000000000000000, -1.031065855027150586E-29, 2.218671295934095703E-30 ) ) ;
#7564 = CARTESIAN_POINT ( 'NONE',  ( 34.00000000000000000, 0.000000000000000000, 1.609999999999982778 ) ) ;
#7565 = CARTESIAN_POINT ( 'NONE',  ( 33.00000000000001421, 39.34792583643766761, -17.06347054209568270 ) ) ;
#7566 = ORIENTED_EDGE ( 'NONE', *, *, #3967, .T. ) ;
#7567 = ADVANCED_FACE ( 'NONE', ( #6663 ), #11428, .T. ) ;
#7568 = CARTESIAN_POINT ( 'NONE',  ( 0.000000000000000000, 5.483475578891660263, -3.488337222187519515 ) ) ;
#7569 = LINE ( 'NONE', #10527, #2917 ) ;
#7570 = VERTEX_POINT ( 'NONE', #11491 ) ;
#7571 = VERTEX_POINT ( 'NONE', #4658 ) ;
#7572 = CYLINDRICAL_SURFACE ( 'NONE', #5533, 6.499000000000010324 ) ;
#7573 = ORIENTED_EDGE ( 'NONE', *, *, #2969, .T. ) ;
#7574 = ORIENTED_EDGE ( 'NONE', *, *, #2637, .F. ) ;
#7575 = CARTESIAN_POINT ( 'NONE',  ( 9.714451465470119729E-14, 0.8865213383406691516, -1.535500000000002085 ) ) ;
#7576 = ORIENTED_EDGE ( 'NONE', *, *, #11338, .F. ) ;
#7577 = EDGE_CURVE ( 'NONE', #7823, #12092, #12466, .T. ) ;
#7578 = CARTESIAN_POINT ( 'NONE',  ( 11.00000000000003730, -19.99999999999999645, 9.850000000000040501 ) ) ;
#7579 = DIRECTION ( 'NONE',  ( 0.000000000000000000, 0.000000000000000000, -1.000000000000000000 ) ) ;
#7580 = VERTEX_POINT ( 'NONE', #10443 ) ;
#7581 = CARTESIAN_POINT ( 'NONE',  ( 33.00000000000000711, 39.92642927056392210, -44.05727230799563898 ) ) ;
#7582 = CARTESIAN_POINT ( 'NONE',  ( 40.00000000000000711, 40.41548023366552655, -10.14535464186970692 ) ) ;
#7583 = AXIS2_PLACEMENT_3D ( 'NONE', #11376, #8462, #2555 ) ;
#7584 = EDGE_CURVE ( 'NONE', #5731, #6619, #3225, .T. ) ;
#7585 = DIRECTION ( 'NONE',  ( -1.000000000000000000, 1.010728034814421376E-30, 1.090846720500930387E-30 ) ) ;
#7586 = EDGE_CURVE ( 'NONE', #9185, #11818, #8122, .T. ) ;
#7587 = ORIENTED_EDGE ( 'NONE', *, *, #9179, .T. ) ;
#7588 = AXIS2_PLACEMENT_3D ( 'NONE', #4, #6050, #9962 ) ;
#7589 = AXIS2_PLACEMENT_3D ( 'NONE', #765, #12503, #3677 ) ;
#7590 = ORIENTED_EDGE ( 'NONE', *, *, #8905, .F. ) ;
#7591 = DIRECTION ( 'NONE',  ( -1.000000000000000000, -1.031065855027150586E-29, 2.218671295934095703E-30 ) ) ;
#7592 = PRODUCT_DEFINITION_SHAPE ( 'NONE', 'NONE',  #12757 ) ;
#7593 = PRESENTATION_LAYER_ASSIGNMENT (  '', '', ( #391 ) ) ;
#7594 = CARTESIAN_POINT ( 'NONE',  ( 44.00000000000000711, 39.34792583643766051, -17.06347054209567915 ) ) ;
#7595 = EDGE_LOOP ( 'NONE', ( #6014, #8254, #11595, #8220 ) ) ;
#7596 = FACE_OUTER_BOUND ( 'NONE', #9405, .T. ) ;
#7597 = CARTESIAN_POINT ( 'NONE',  ( 33.00000000000001421, 81.84122341717352356, -27.68198508464163510 ) ) ;
#7598 = CIRCLE ( 'NONE', #11101, 2.800000000000003819 ) ;
#7599 = CIRCLE ( 'NONE', #2470, 2.800000000000003375 ) ;
#7600 = CARTESIAN_POINT ( 'NONE',  ( 0.000000000000000000, 0.000000000000000000, 0.000000000000000000 ) ) ;
#7601 = VECTOR ( 'NONE', #7665, 1000.000000000000000 ) ;
#7602 = EDGE_CURVE ( 'NONE', #1279, #6823, #8512, .T. ) ;
#7603 = DIRECTION ( 'NONE',  ( 0.000000000000000000, 0.000000000000000000, -1.000000000000000000 ) ) ;
#7604 = VERTEX_POINT ( 'NONE', #1034 ) ;
#7605 = DIRECTION ( 'NONE',  ( 0.000000000000000000, -1.177425296209236209E-30, -1.000000000000000000 ) ) ;
#7606 = EDGE_LOOP ( 'NONE', ( #4541, #7858, #8807, #7282 ) ) ;
#7607 = CARTESIAN_POINT ( 'NONE',  ( 0.000000000000000000, -5.148708580507714849, 3.965829163366255017 ) ) ;
#7608 = AXIS2_PLACEMENT_3D ( 'NONE', #9067, #11985, #7088 ) ;
#7609 = AXIS2_PLACEMENT_3D ( 'NONE', #1420, #11087, #4324 ) ;
#7610 = AXIS2_PLACEMENT_3D ( 'NONE', #12084, #11961, #12021 ) ;
#7611 = EDGE_CURVE ( 'NONE', #865, #12067, #6500, .T. ) ;
#7612 = DIRECTION ( 'NONE',  ( 0.000000000000000000, 0.000000000000000000, 1.000000000000000000 ) ) ;
#7613 = LINE ( 'NONE', #1558, #8689 ) ;
#7614 = DIRECTION ( 'NONE',  ( 1.000000000000000000, -6.162975822039154730E-33, -4.563833282352349791E-17 ) ) ;
#7615 = CARTESIAN_POINT ( 'NONE',  ( -11.83215956619923226, 30.00000000000000000, -4.336808689942017736E-16 ) ) ;
#7616 = DIRECTION ( 'NONE',  ( -1.000000000000000000, 0.000000000000000000, 1.224646799147352714E-16 ) ) ;
#7617 = DIRECTION ( 'NONE',  ( -1.000000000000000000, 1.010728034814421376E-30, 1.090846720500930387E-30 ) ) ;
#7618 = VECTOR ( 'NONE', #7526, 1000.000000000000114 ) ;
#7619 = AXIS2_PLACEMENT_3D ( 'NONE', #9421, #9488, #5454 ) ;
#7620 = EDGE_CURVE ( 'NONE', #9518, #9949, #1937, .T. ) ;
#7621 = DIRECTION ( 'NONE',  ( 0.000000000000000000, -1.530455820933490821E-32, 1.000000000000000000 ) ) ;
#7622 = PRODUCT_DEFINITION_SHAPE ( 'NONE', 'NONE',  #6898 ) ;
#7623 = EDGE_CURVE ( 'NONE', #3861, #5717, #9844, .T. ) ;
#7624 = DIRECTION ( 'NONE',  ( -1.000000000000000000, 1.010728034814421376E-30, 1.090846720500930387E-30 ) ) ;
#7625 = CARTESIAN_POINT ( 'NONE',  ( 0.000000000000000000, 6.057062246029517816, 4.251117141143491374 ) ) ;
#7626 = ORIENTED_EDGE ( 'NONE', *, *, #11251, .F. ) ;
#7627 = EDGE_CURVE ( 'NONE', #6234, #3861, #7923, .T. ) ;
#7628 = STYLED_ITEM ( 'NONE', ( #2064 ), #6187 ) ;
#7629 = ORIENTED_EDGE ( 'NONE', *, *, #10619, .F. ) ;
#7630 = ORIENTED_EDGE ( 'NONE', *, *, #666, .T. ) ;
#7631 = LINE ( 'NONE', #8720, #1919 ) ;
#7632 = CARTESIAN_POINT ( 'NONE',  ( 19.99999999999999645, 5.012092988313947117, 4.137139697483554812 ) ) ;
#7633 = CARTESIAN_POINT ( 'NONE',  ( 11.17157287525379772, 30.00000000000000000, -2.828427124746177856 ) ) ;
#7634 = CARTESIAN_POINT ( 'NONE',  ( 40.00000000000000711, 8.524480296082934672, -16.78569723734484143 ) ) ;
#7635 = ORIENTED_EDGE ( 'NONE', *, *, #10367, .T. ) ;
#7636 = DIRECTION ( 'NONE',  ( 0.000000000000000000, 0.000000000000000000, -1.000000000000000000 ) ) ;
#7637 =( GEOMETRIC_REPRESENTATION_CONTEXT ( 3 ) GLOBAL_UNCERTAINTY_ASSIGNED_CONTEXT ( ( #8550 ) ) GLOBAL_UNIT_ASSIGNED_CONTEXT ( ( #9200, #1476, #5220 ) ) REPRESENTATION_CONTEXT ( 'NONE', 'WORKASPACE' ) );
#7638 = LINE ( 'NONE', #2827, #1853 ) ;
#7639 = ORIENTED_EDGE ( 'NONE', *, *, #5621, .T. ) ;
#7640 = ORIENTED_EDGE ( 'NONE', *, *, #706, .F. ) ;
#7641 = CARTESIAN_POINT ( 'NONE',  ( 2.000000000000001776, -0.8865213383406691516, 1.535500000000002085 ) ) ;
#7642 = ORIENTED_EDGE ( 'NONE', *, *, #12431, .T. ) ;
#7643 = ORIENTED_EDGE ( 'NONE', *, *, #10429, .T. ) ;
#7644 =( NAMED_UNIT ( * ) SI_UNIT ( $, .STERADIAN. ) SOLID_ANGLE_UNIT ( ) );
#7645 = CYLINDRICAL_SURFACE ( 'NONE', #11723, 7.400000000000010125 ) ;
#7646 = ORIENTED_EDGE ( 'NONE', *, *, #1641, .T. ) ;
#7647 = AXIS2_PLACEMENT_3D ( 'NONE', #1810, #5739, #2741 ) ;
#7648 = LINE ( 'NONE', #1658, #8817 ) ;
#7649 = CARTESIAN_POINT ( 'NONE',  ( 14.00000000000000000, -12.99999999999999822, -4.000000000000000000 ) ) ;
#7650 = AXIS2_PLACEMENT_3D ( 'NONE', #10907, #2095, #7494 ) ;
#7651 = ORIENTED_EDGE ( 'NONE', *, *, #11184, .F. ) ;
#7652 = CARTESIAN_POINT ( 'NONE',  ( 10.00000000000000178, 6.718789039999964352, 3.101269713516805027 ) ) ;
#7653 = CYLINDRICAL_SURFACE ( 'NONE', #6477, 2.800000000000003819 ) ;
#7654 = ORIENTED_EDGE ( 'NONE', *, *, #10502, .F. ) ;
#7655 = ORIENTED_EDGE ( 'NONE', *, *, #9778, .F. ) ;
#7656 = VECTOR ( 'NONE', #1294, 1000.000000000000000 ) ;
#7657 = EDGE_LOOP ( 'NONE', ( #10075, #10263, #6351, #9047, #7364 ) ) ;
#7658 =( REPRESENTATION_RELATIONSHIP ('NONE','NONE', #10018, #891 ) REPRESENTATION_RELATIONSHIP_WITH_TRANSFORMATION ( #5436 )SHAPE_REPRESENTATION_RELATIONSHIP( ) );
#7659 = PLANE ( 'NONE',  #1498 ) ;
#7660 = CARTESIAN_POINT ( 'NONE',  ( 46.00000000000009237, -20.00000000000013500, -11.99999999999951150 ) ) ;
#7661 = ORIENTED_EDGE ( 'NONE', *, *, #2067, .T. ) ;
#7662 = ADVANCED_FACE ( 'NONE', ( #848 ), #5929, .T. ) ;
#7663 = CARTESIAN_POINT ( 'NONE',  ( 3.680118525130243956, -2.494084732383345493, -0.3507732604232523532 ) ) ;
#7664 = CLOSED_SHELL ( 'NONE', ( #11318, #8093, #726, #9848, #3123, #7850, #9969, #11541, #1667, #10336, #5078 ) ) ;
#7665 = DIRECTION ( 'NONE',  ( -1.000000000000000000, 1.010728034814421376E-30, 1.090846720500930387E-30 ) ) ;
#7666 = AXIS2_PLACEMENT_3D ( 'NONE', #10352, #575, #12500 ) ;
#7667 = CARTESIAN_POINT ( 'NONE',  ( -4.197393957002295117, -8.025123413315649349E-14, -3.503767560748944021 ) ) ;
#7668 = CARTESIAN_POINT ( 'NONE',  ( 0.000000000000000000, 4.618802153517012954, -5.000000000000018652 ) ) ;
#7669 = ORIENTED_EDGE ( 'NONE', *, *, #5969, .F. ) ;
#7670 = DIRECTION ( 'NONE',  ( 0.000000000000000000, 0.000000000000000000, 1.000000000000000000 ) ) ;
#7671 = ORIENTED_EDGE ( 'NONE', *, *, #3163, .T. ) ;
#7672 = AXIS2_PLACEMENT_3D ( 'NONE', #2540, #4593, #1687 ) ;
#7673 = CARTESIAN_POINT ( 'NONE',  ( -31.74999999999995026, 0.000000000000000000, -1.734723475976807094E-14 ) ) ;
#7674 = AXIS2_PLACEMENT_3D ( 'NONE', #10610, #7591, #4509 ) ;
#7675 = LINE ( 'NONE', #650, #1425 ) ;
#7676 = EDGE_CURVE ( 'NONE', #4250, #8666, #10633, .T. ) ;
#7677 = PRODUCT_RELATED_PRODUCT_CATEGORY ( 'part', '', ( #4427 ) ) ;
#7678 = CYLINDRICAL_SURFACE ( 'NONE', #11997, 7.400000000000010125 ) ;
#7679 = DIRECTION ( 'NONE',  ( 0.000000000000000000, 0.000000000000000000, 1.000000000000000000 ) ) ;
#7680 = CIRCLE ( 'NONE', #1089, 7.400000000000009237 ) ;
#7681 = CARTESIAN_POINT ( 'NONE',  ( -10.00000000000000178, 0.000000000000000000, 0.000000000000000000 ) ) ;
#7682 = DIRECTION ( 'NONE',  ( 1.133987551255203244E-30, -0.9909497617679332571, -0.1342332658176667859 ) ) ;
#7683 = DIRECTION ( 'NONE',  ( 0.000000000000000000, 1.000000000000000000, 0.000000000000000000 ) ) ;
#7684 = CARTESIAN_POINT ( 'NONE',  ( 0.000000000000000000, -6.310777386698730673, 1.552768423021301469 ) ) ;
#7685 = CARTESIAN_POINT ( 'NONE',  ( 14.00000000000000000, 30.00000000000000000, 0.000000000000000000 ) ) ;
#7686 = CARTESIAN_POINT ( 'NONE',  ( 9.999999999999994671, -5.651611091574839207, 4.776954267060578019 ) ) ;
#7687 = ORIENTED_EDGE ( 'NONE', *, *, #6963, .F. ) ;
#7688 = VERTEX_POINT ( 'NONE', #9784 ) ;
#7689 = EDGE_CURVE ( 'NONE', #10242, #10664, #2375, .T. ) ;
#7690 = ORIENTED_EDGE ( 'NONE', *, *, #1595, .F. ) ;
#7691 = CARTESIAN_POINT ( 'NONE',  ( 14.00000000000000000, -30.00000000000000000, 3.999999999999997335 ) ) ;
#7692 = EDGE_CURVE ( 'NONE', #11033, #11719, #5804, .T. ) ;
#7693 = CARTESIAN_POINT ( 'NONE',  ( 4.000000000000000000, -1.560351142792954171, -0.2242961665059817755 ) ) ;
#7694 = FACE_OUTER_BOUND ( 'NONE', #10865, .T. ) ;
#7695 = LINE ( 'NONE', #8662, #11660 ) ;
#7696 = EDGE_LOOP ( 'NONE', ( #3992, #316, #11782, #7372, #12487, #728, #7706, #5957, #2852, #6384, #6115, #11761, #12105, #10125, #5202, #7330, #8038, #6402, #7020, #9537, #4441, #12616 ) ) ;
#7697 = CIRCLE ( 'NONE', #11201, 24.99999999999998934 ) ;
#7698 = DIRECTION ( 'NONE',  ( 0.000000000000000000, -1.530455820933490821E-32, 1.000000000000000000 ) ) ;
#7699 = AXIS2_PLACEMENT_3D ( 'NONE', #465, #6462, #6324 ) ;
#7700 = EDGE_CURVE ( 'NONE', #3671, #5846, #912, .T. ) ;
#7701 = ORIENTED_EDGE ( 'NONE', *, *, #9385, .T. ) ;
#7702 = ORIENTED_EDGE ( 'NONE', *, *, #1676, .F. ) ;
#7703 = DIRECTION ( 'NONE',  ( 2.465190328815656418E-32, -1.177425296209236734E-30, -1.000000000000000000 ) ) ;
#7704 = EDGE_LOOP ( 'NONE', ( #7346, #3157, #7106, #6443 ) ) ;
#7705 = CIRCLE ( 'NONE', #2149, 7.400000000000009237 ) ;
#7706 = ORIENTED_EDGE ( 'NONE', *, *, #925, .T. ) ;
#7707 = VECTOR ( 'NONE', #1436, 1000.000000000000000 ) ;
#7708 = FILL_AREA_STYLE_COLOUR ( '', #209 ) ;
#7709 = DIRECTION ( 'NONE',  ( 0.000000000000000000, 0.000000000000000000, 1.000000000000000000 ) ) ;
#7710 = ORIENTED_EDGE ( 'NONE', *, *, #6579, .F. ) ;
#7711 = ADVANCED_FACE ( 'NONE', ( #3821 ), #2004, .T. ) ;
#7712 = DIRECTION ( 'NONE',  ( -1.000000000000000000, 0.000000000000000000, 0.000000000000000000 ) ) ;
#7713 = EDGE_CURVE ( 'NONE', #1584, #6210, #4629, .T. ) ;
#7714 = CARTESIAN_POINT ( 'NONE',  ( 14.00000000000000000, 12.99999999999999822, 0.000000000000000000 ) ) ;
#7715 = ORIENTED_EDGE ( 'NONE', *, *, #2925, .F. ) ;
#7716 = DIRECTION ( 'NONE',  ( -2.465190328815656418E-32, 1.177425296209236734E-30, 1.000000000000000000 ) ) ;
#7717 = CARTESIAN_POINT ( 'NONE',  ( 2.000000000000001776, 0.000000000000000000, 1.535500000000002085 ) ) ;
#7718 = CIRCLE ( 'NONE', #11219, 2.800000000000004263 ) ;
#7719 = AXIS2_PLACEMENT_3D ( 'NONE', #8742, #4628, #10478 ) ;
#7720 = VERTEX_POINT ( 'NONE', #2808 ) ;
#7721 = ORIENTED_EDGE ( 'NONE', *, *, #3132, .T. ) ;
#7722 = VERTEX_POINT ( 'NONE', #11613 ) ;
#7723 = CARTESIAN_POINT ( 'NONE',  ( 19.99999999999999645, 0.000000000000000000, 0.000000000000000000 ) ) ;
#7724 = CIRCLE ( 'NONE', #10382, 7.400000000000009237 ) ;
#7725 = DIRECTION ( 'NONE',  ( 6.982962677686266711E-15, 0.000000000000000000, -1.000000000000000000 ) ) ;
#7726 = ORIENTED_EDGE ( 'NONE', *, *, #11568, .F. ) ;
#7727 = VECTOR ( 'NONE', #1829, 1000.000000000000114 ) ;
#7728 = CARTESIAN_POINT ( 'NONE',  ( 19.99999999999999645, -1.966014849757073968, 6.277170897746257694 ) ) ;
#7729 = VERTEX_POINT ( 'NONE', #4907 ) ;
#7730 = LINE ( 'NONE', #4829, #7601 ) ;
#7731 = EDGE_CURVE ( 'NONE', #11454, #2770, #5437, .T. ) ;
#7732 = EDGE_CURVE ( 'NONE', #11692, #927, #1964, .T. ) ;
#7733 = CARTESIAN_POINT ( 'NONE',  ( 0.5276280594148604619, -4.314175951381856500, -3.320322319202345440 ) ) ;
#7734 = TOROIDAL_SURFACE ( 'NONE', #2816, 3.299999999999999822, 0.2000000000000000111 ) ;
#7735 = LINE ( 'NONE', #9829, #350 ) ;
#7736 = ORIENTED_EDGE ( 'NONE', *, *, #8947, .T. ) ;
#7737 = CARTESIAN_POINT ( 'NONE',  ( 4.000000000000002665, 2.309401076758486937, -3.504271511727107047 ) ) ;
#7738 = ORIENTED_EDGE ( 'NONE', *, *, #4984, .T. ) ;
#7739 = CARTESIAN_POINT ( 'NONE',  ( 0.000000000000000000, 1.052479792859058128, 6.413211932068317189 ) ) ;
#7740 = CARTESIAN_POINT ( 'NONE',  ( 0.000000000000000000, -3.178467454237101197, -5.758943784352613449 ) ) ;
#7741 = CIRCLE ( 'NONE', #8380, 5.384454397937118664 ) ;
#7742 = CARTESIAN_POINT ( 'NONE',  ( 0.000000000000000000, 0.000000000000000000, 0.000000000000000000 ) ) ;
#7743 = DIRECTION ( 'NONE',  ( -1.000000000000000000, 1.010728034814421376E-30, 1.090846720500930387E-30 ) ) ;
#7744 = CARTESIAN_POINT ( 'NONE',  ( 15.00000000000003375, 30.00000000000001776, -6.000000000000013323 ) ) ;
#7745 = CARTESIAN_POINT ( 'NONE',  ( 19.99999999999999645, 0.000000000000000000, 0.000000000000000000 ) ) ;
#7746 = CARTESIAN_POINT ( 'NONE',  ( -9.860132971832690885, 30.00000000000000000, -1.666666666666667629 ) ) ;
#7747 = DIRECTION ( 'NONE',  ( -1.000000000000000000, 1.006188713385347367E-17, 3.844790828812615713E-17 ) ) ;
#7748 = EDGE_CURVE ( 'NONE', #10993, #11393, #1938, .T. ) ;
#7749 = EDGE_CURVE ( 'NONE', #11074, #1327, #12649, .T. ) ;
#7750 = EDGE_CURVE ( 'NONE', #10716, #3178, #10755, .T. ) ;
#7751 = AXIS2_PLACEMENT_3D ( 'NONE', #6674, #2946, #3771 ) ;
#7752 = EDGE_CURVE ( 'NONE', #2092, #10338, #1532, .T. ) ;
#7753 = PLANE ( 'NONE',  #32 ) ;
#7754 = EDGE_LOOP ( 'NONE', ( #2195, #9692, #9931, #1764 ) ) ;
#7755 = ORIENTED_EDGE ( 'NONE', *, *, #5822, .T. ) ;
#7756 = FACE_OUTER_BOUND ( 'NONE', #636, .T. ) ;
#7757 = DIRECTION ( 'NONE',  ( 2.465190328815656418E-32, -1.177425296209236734E-30, -1.000000000000000000 ) ) ;
#7758 = DIRECTION ( 'NONE',  ( -1.000000000000000000, 1.010728034814421376E-30, 1.090846720500930387E-30 ) ) ;
#7759 = DIRECTION ( 'NONE',  ( 1.000000000000000000, 1.031065855027150586E-29, 2.218671295934092550E-30 ) ) ;
#7760 = ORIENTED_EDGE ( 'NONE', *, *, #2247, .F. ) ;
#7761 = CIRCLE ( 'NONE', #8785, 2.800000000000004263 ) ;
#7762 = DIRECTION ( 'NONE',  ( -1.000000000000000000, 0.000000000000000000, 0.000000000000000000 ) ) ;
#7763 = DIRECTION ( 'NONE',  ( -1.000000000000000000, 1.010728034814421376E-30, 1.090846720500930387E-30 ) ) ;
#7764 = ORIENTED_EDGE ( 'NONE', *, *, #3539, .T. ) ;
#7765 = EDGE_LOOP ( 'NONE', ( #6606, #10341, #12356, #9360 ) ) ;
#7766 = DIRECTION ( 'NONE',  ( 0.000000000000000000, -1.000000000000000000, 0.000000000000000000 ) ) ;
#7767 = ORIENTED_EDGE ( 'NONE', *, *, #4151, .F. ) ;
#7768 = ORIENTED_EDGE ( 'NONE', *, *, #10599, .F. ) ;
#7769 = VECTOR ( 'NONE', #7133, 1000.000000000000114 ) ;
#7770 = LINE ( 'NONE', #3724, #6156 ) ;
#7771 = ORIENTED_EDGE ( 'NONE', *, *, #3381, .T. ) ;
#7772 = DIRECTION ( 'NONE',  ( -1.000000000000000000, 1.010728034814421376E-30, 1.090846720500930387E-30 ) ) ;
#7773 = EDGE_CURVE ( 'NONE', #12678, #10836, #8954, .T. ) ;
#7774 = CARTESIAN_POINT ( 'NONE',  ( 19.99999999999997868, -1.268072931708450257, -6.374087545670231947 ) ) ;
#7775 = VERTEX_POINT ( 'NONE', #7165 ) ;
#7776 = CARTESIAN_POINT ( 'NONE',  ( 4.000000000000003553, 3.499999999999999556, 0.000000000000000000 ) ) ;
#7777 = ADVANCED_FACE ( 'NONE', ( #10221 ), #7983, .T. ) ;
#7778 = DIRECTION ( 'NONE',  ( 1.000000000000000000, 1.849040895279789448E-31, -6.938893903907224680E-17 ) ) ;
#7779 = ADVANCED_FACE ( 'NONE', ( #11933 ), #10102, .F. ) ;
#7780 = ORIENTED_EDGE ( 'NONE', *, *, #4969, .F. ) ;
#7781 = ORIENTED_EDGE ( 'NONE', *, *, #183, .T. ) ;
#7782 = EDGE_CURVE ( 'NONE', #8600, #11206, #9743, .T. ) ;
#7783 = EDGE_LOOP ( 'NONE', ( #2714, #7895, #788, #7640 ) ) ;
#7784 = DIRECTION ( 'NONE',  ( 1.000000000000000000, -1.010728034814421376E-30, -1.090846720500930387E-30 ) ) ;
#7785 = ORIENTED_EDGE ( 'NONE', *, *, #10041, .F. ) ;
#7786 = DIRECTION ( 'NONE',  ( 0.000000000000000000, 0.000000000000000000, 1.000000000000000000 ) ) ;
#7787 = ORIENTED_EDGE ( 'NONE', *, *, #11606, .T. ) ;
#7788 = DIRECTION ( 'NONE',  ( 0.000000000000000000, 0.000000000000000000, -1.000000000000000000 ) ) ;
#7789 = DIRECTION ( 'NONE',  ( -1.000000000000000000, 1.010728034814421376E-30, 1.090846720500930387E-30 ) ) ;
#7790 = DIRECTION ( 'NONE',  ( 0.000000000000000000, -0.9749279121818259508, 0.2225209339563040400 ) ) ;
#7791 = ORIENTED_EDGE ( 'NONE', *, *, #10234, .F. ) ;
#7792 = VECTOR ( 'NONE', #3400, 1000.000000000000000 ) ;
#7793 = CARTESIAN_POINT ( 'NONE',  ( 27.00000000000001421, 81.84122341717352356, -52.68198508464163154 ) ) ;
#7794 = ORIENTED_EDGE ( 'NONE', *, *, #296, .T. ) ;
#7795 = CARTESIAN_POINT ( 'NONE',  ( -18.00000000000000355, 29.99999999999998224, 3.000000000000008438 ) ) ;
#7796 = EDGE_CURVE ( 'NONE', #9165, #276, #9205, .T. ) ;
#7797 = FACE_OUTER_BOUND ( 'NONE', #6743, .T. ) ;
#7798 = AXIS2_PLACEMENT_3D ( 'NONE', #11221, #10222, #5351 ) ;
#7799 = AXIS2_PLACEMENT_3D ( 'NONE', #6892, #10801, #1982 ) ;
#7800 = AXIS2_PLACEMENT_3D ( 'NONE', #6724, #7624, #10510 ) ;
#7801 = LINE ( 'NONE', #6779, #8674 ) ;
#7802 = AXIS2_PLACEMENT_3D ( 'NONE', #11581, #8672, #5768 ) ;
#7803 = CARTESIAN_POINT ( 'NONE',  ( -14.99999999999999289, 30.00000000000000000, 25.00000000000007105 ) ) ;
#7804 = DIRECTION ( 'NONE',  ( -1.159061634649218351E-16, 0.000000000000000000, -1.000000000000000000 ) ) ;
#7805 = DIRECTION ( 'NONE',  ( 0.000000000000000000, -1.000000000000000000, 0.000000000000000000 ) ) ;
#7806 = DIRECTION ( 'NONE',  ( -0.000000000000000000, -1.000000000000000000, -0.000000000000000000 ) ) ;
#7807 = CARTESIAN_POINT ( 'NONE',  ( 3.122502256758252770E-14, -4.862606272033112909, -3.745885042887444616 ) ) ;
#7808 = CIRCLE ( 'NONE', #12345, 2.800000000000003819 ) ;
#7809 = AXIS2_PLACEMENT_3D ( 'NONE', #11548, #12511, #5548 ) ;
#7810 = AXIS2_PLACEMENT_3D ( 'NONE', #10628, #3752, #8642 ) ;
#7811 = CARTESIAN_POINT ( 'NONE',  ( 9.999999999999994671, -2.401522331692915735, 6.999477872697376313 ) ) ;
#7812 = ORIENTED_EDGE ( 'NONE', *, *, #12574, .F. ) ;
#7813 = ORIENTED_EDGE ( 'NONE', *, *, #6843, .F. ) ;
#7814 = EDGE_CURVE ( 'NONE', #5068, #5859, #5100, .T. ) ;
#7815 = CARTESIAN_POINT ( 'NONE',  ( 19.99999999999997868, 6.321830586517925177, 1.817291089601345888 ) ) ;
#7816 = AXIS2_PLACEMENT_3D ( 'NONE', #616, #11444, #12608 ) ;
#7817 = DIRECTION ( 'NONE',  ( 2.206345344290014591E-30, -7.771561172376086908E-16, -1.000000000000000000 ) ) ;
#7819 = ADVANCED_FACE ( 'NONE', ( #12061 ), #1225, .F. ) ;
#7818 = FACE_OUTER_BOUND ( 'NONE', #5526, .T. ) ;
#7820 = AXIS2_PLACEMENT_3D ( 'NONE', #991, #6621, #744 ) ;
#7821 = AXIS2_PLACEMENT_3D ( 'NONE', #11407, #2586, #6512 ) ;
#7822 = CARTESIAN_POINT ( 'NONE',  ( 19.99999999999999645, 0.000000000000000000, 0.000000000000000000 ) ) ;
#7823 = VERTEX_POINT ( 'NONE', #261 ) ;
#7824 = LINE ( 'NONE', #2948, #3213 ) ;
#7825 = FACE_OUTER_BOUND ( 'NONE', #7274, .T. ) ;
#7826 = DIRECTION ( 'NONE',  ( -0.7071067811865504593, 0.000000000000000000, -0.7071067811865445751 ) ) ;
#7827 = ORIENTED_EDGE ( 'NONE', *, *, #537, .T. ) ;
#7828 = ORIENTED_EDGE ( 'NONE', *, *, #8344, .T. ) ;
#7829 = DIRECTION ( 'NONE',  ( 1.000000000000000000, 0.000000000000000000, -2.168404344971007882E-16 ) ) ;
#7830 = EDGE_LOOP ( 'NONE', ( #4234, #12300 ) ) ;
#7831 = VECTOR ( 'NONE', #7826, 1000.000000000000000 ) ;
#7832 = ORIENTED_EDGE ( 'NONE', *, *, #4682, .F. ) ;
#7833 = DIRECTION ( 'NONE',  ( 0.000000000000000000, -1.530455820933490821E-32, 1.000000000000000000 ) ) ;
#7834 = ORIENTED_EDGE ( 'NONE', *, *, #306, .T. ) ;
#7835 = FACE_OUTER_BOUND ( 'NONE', #6870, .T. ) ;
#7836 = DIRECTION ( 'NONE',  ( -1.000000000000000000, 1.010728034814421376E-30, 1.090846720500930387E-30 ) ) ;
#7837 = EDGE_CURVE ( 'NONE', #10019, #1407, #1351, .T. ) ;
#7838 = ORIENTED_EDGE ( 'NONE', *, *, #6412, .F. ) ;
#7839 = LINE ( 'NONE', #7892, #7159 ) ;
#7840 = FACE_OUTER_BOUND ( 'NONE', #380, .T. ) ;
#7841 = STYLED_ITEM ( 'NONE', ( #5030 ), #1117 ) ;
#7842 = ORIENTED_EDGE ( 'NONE', *, *, #3054, .T. ) ;
#7843 = ORIENTED_EDGE ( 'NONE', *, *, #2110, .F. ) ;
#7844 = VERTEX_POINT ( 'NONE', #390 ) ;
#7845 = PLANE ( 'NONE',  #12409 ) ;
#7846 = CIRCLE ( 'NONE', #9275, 7.400000000000011902 ) ;
#7847 = ORIENTED_EDGE ( 'NONE', *, *, #8344, .F. ) ;
#7848 = FACE_OUTER_BOUND ( 'NONE', #7943, .T. ) ;
#7849 = ORIENTED_EDGE ( 'NONE', *, *, #895, .T. ) ;
#7850 = ADVANCED_FACE ( 'NONE', ( #6059 ), #3186, .T. ) ;
#7851 = ADVANCED_FACE ( 'NONE', ( #4321 ), #12191, .F. ) ;
#7852 = FACE_OUTER_BOUND ( 'NONE', #7048, .T. ) ;
#7853 = AXIS2_PLACEMENT_3D ( 'NONE', #459, #9209, #7168 ) ;
#7854 = CARTESIAN_POINT ( 'NONE',  ( 14.00000000000000000, 30.00000000000000000, -6.000000000000000000 ) ) ;
#7855 = ADVANCED_FACE ( 'NONE', ( #5350 ), #4194, .T. ) ;
#7856 = ORIENTED_EDGE ( 'NONE', *, *, #6065, .T. ) ;
#7857 = CARTESIAN_POINT ( 'NONE',  ( 19.99999999999999645, 3.681899619563770543, 5.450844343808956438 ) ) ;
#7858 = ORIENTED_EDGE ( 'NONE', *, *, #3637, .T. ) ;
#7859 = CARTESIAN_POINT ( 'NONE',  ( -3.999999999999970690, -2.309401076758515359, -5.000000000000018652 ) ) ;
#7860 = DIRECTION ( 'NONE',  ( -1.000000000000000000, 1.010728034814421376E-30, 1.090846720500930387E-30 ) ) ;
#7861 = VECTOR ( 'NONE', #8366, 1000.000000000000000 ) ;
#7862 = DIRECTION ( 'NONE',  ( -1.000000000000000000, 1.010728034814421376E-30, 1.090846720500930387E-30 ) ) ;
#7863 = DIRECTION ( 'NONE',  ( 1.140150527077241873E-30, 0.000000000000000000, -1.000000000000000000 ) ) ;
#7864 = DIRECTION ( 'NONE',  ( -1.000000000000000000, 1.010728034814421376E-30, 1.090846720500930387E-30 ) ) ;
#7865 = CARTESIAN_POINT ( 'NONE',  ( -3.999999999999991562, -1.560351142792946622, -0.2242961665059734766 ) ) ;
#7866 = DIRECTION ( 'NONE',  ( 1.000000000000000000, -1.010728034814421376E-30, -1.090846720500930387E-30 ) ) ;
#7867 = CIRCLE ( 'NONE', #5609, 2.149999999999994138 ) ;
#7868 = CIRCLE ( 'NONE', #11589, 2.800000000000004263 ) ;
#7869 = PLANE ( 'NONE',  #196 ) ;
#7870 = DIRECTION ( 'NONE',  ( 1.000000000000000000, -0.000000000000000000, -6.938893903907228378E-17 ) ) ;
#7871 = ORIENTED_EDGE ( 'NONE', *, *, #6913, .F. ) ;
#7872 = DIRECTION ( 'NONE',  ( -6.532754371361493504E-31, 0.9510565162951545304, -0.3090169943749445092 ) ) ;
#7873 = CYLINDRICAL_SURFACE ( 'NONE', #6453, 6.499000000000010324 ) ;
#7874 = FACE_OUTER_BOUND ( 'NONE', #935, .T. ) ;
#7875 = DIRECTION ( 'NONE',  ( 0.000000000000000000, 0.000000000000000000, 1.000000000000000000 ) ) ;
#7876 = PLANE ( 'NONE',  #6928 ) ;
#7877 = ORIENTED_EDGE ( 'NONE', *, *, #12321, .F. ) ;
#7878 = CYLINDRICAL_SURFACE ( 'NONE', #7510, 2.149999999999999023 ) ;
#7879 = CARTESIAN_POINT ( 'NONE',  ( 4.000000000000001776, 2.309401076758487381, -3.433295621305364254 ) ) ;
#7880 = DIRECTION ( 'NONE',  ( -1.000000000000000000, -1.081682119347366197E-16, 6.938893903907228378E-17 ) ) ;
#7881 = ORIENTED_EDGE ( 'NONE', *, *, #269, .T. ) ;
#7882 = AXIS2_PLACEMENT_3D ( 'NONE', #6980, #2148, #6001 ) ;
#7883 = VERTEX_POINT ( 'NONE', #2208 ) ;
#7884 = CYLINDRICAL_SURFACE ( 'NONE', #10513, 2.800000000000003819 ) ;
#7885 = ORIENTED_EDGE ( 'NONE', *, *, #527, .F. ) ;
#7886 = ORIENTED_EDGE ( 'NONE', *, *, #3433, .T. ) ;
#7887 = DIRECTION ( 'NONE',  ( -1.000000000000000000, -1.031065855027150586E-29, 2.218671295934095703E-30 ) ) ;
#7888 = ORIENTED_EDGE ( 'NONE', *, *, #5324, .T. ) ;
#7889 = DIRECTION ( 'NONE',  ( -1.000000000000000000, 6.162975822039154730E-33, 4.563833282352349791E-17 ) ) ;
#7890 = ORIENTED_EDGE ( 'NONE', *, *, #12582, .F. ) ;
#7891 = CIRCLE ( 'NONE', #1730, 6.499000000000009436 ) ;
#7892 = CARTESIAN_POINT ( 'NONE',  ( -31.74999999999995026, 1.942890293094023946E-16, 3.500000000000011102 ) ) ;
#7893 = CARTESIAN_POINT ( 'NONE',  ( 14.00000000000000000, 49.63999999999998636, -5.000000000000001776 ) ) ;
#7894 = AXIS2_PLACEMENT_3D ( 'NONE', #8132, #4146, #11233 ) ;
#7895 = ORIENTED_EDGE ( 'NONE', *, *, #11006, .T. ) ;
#7896 = ADVANCED_FACE ( 'NONE', ( #2272 ), #7034, .T. ) ;
#7897 = ORIENTED_EDGE ( 'NONE', *, *, #2520, .T. ) ;
#7898 = EDGE_CURVE ( 'NONE', #5309, #4808, #11443, .T. ) ;
#7899 = EDGE_CURVE ( 'NONE', #335, #8684, #710, .T. ) ;
#7900 = ORIENTED_EDGE ( 'NONE', *, *, #8716, .T. ) ;
#7901 = CARTESIAN_POINT ( 'NONE',  ( 3.122502256758252770E-14, -4.618802153517027165, -3.433295621305388678 ) ) ;
#7902 = EDGE_LOOP ( 'NONE', ( #11658, #10742, #2316, #5320, #12745 ) ) ;
#7903 = FACE_OUTER_BOUND ( 'NONE', #12102, .T. ) ;
#7904 = ORIENTED_EDGE ( 'NONE', *, *, #3180, .T. ) ;
#7905 = AXIS2_PLACEMENT_3D ( 'NONE', #9142, #328, #10949 ) ;
#7906 = AXIS2_PLACEMENT_3D ( 'NONE', #1852, #9687, #881 ) ;
#7907 = CIRCLE ( 'NONE', #278, 6.999999999999999112 ) ;
#7908 = LINE ( 'NONE', #9577, #6273 ) ;
#7909 = FACE_OUTER_BOUND ( 'NONE', #1040, .T. ) ;
#7910 = ORIENTED_EDGE ( 'NONE', *, *, #6884, .T. ) ;
#7911 = CARTESIAN_POINT ( 'NONE',  ( 2.000000000000091926, 0.000000000000000000, -1.535499999999998755 ) ) ;
#7912 = CIRCLE ( 'NONE', #1123, 7.400000000000009237 ) ;
#7913 = ORIENTED_EDGE ( 'NONE', *, *, #12574, .T. ) ;
#7914 = AXIS2_PLACEMENT_3D ( 'NONE', #4487, #3715, #9605 ) ;
#7915 = CYLINDRICAL_SURFACE ( 'NONE', #7455, 2.800000000000003819 ) ;
#7916 = SURFACE_STYLE_FILL_AREA ( #4123 ) ;
#7917 = DIRECTION ( 'NONE',  ( 0.000000000000000000, -0.4999999999999992784, 0.8660254037844389297 ) ) ;
#7918 = AXIS2_PLACEMENT_3D ( 'NONE', #8372, #12248, #2395 ) ;
#7919 = DIRECTION ( 'NONE',  ( -3.260214209858708648E-30, -0.5000000000000012212, -0.8660254037844380415 ) ) ;
#7920 = ADVANCED_FACE ( 'NONE', ( #2336 ), #7232, .T. ) ;
#7921 = CYLINDRICAL_SURFACE ( 'NONE', #9332, 2.800000000000003819 ) ;
#7922 = CARTESIAN_POINT ( 'NONE',  ( -30.00000000000000000, -30.00000000000000000, 2.000000000000001776 ) ) ;
#7923 = CIRCLE ( 'NONE', #2392, 2.000000000000000888 ) ;
#7924 = CARTESIAN_POINT ( 'NONE',  ( 33.00000000000000000, 29.58047730022061472, -27.90351864933187898 ) ) ;
#7925 = CARTESIAN_POINT ( 'NONE',  ( 19.99999999999997868, 4.192831774279055068, -4.965597920955358902 ) ) ;
#7926 = DIRECTION ( 'NONE',  ( -1.000000000000000000, 0.000000000000000000, 0.000000000000000000 ) ) ;
#7927 = EDGE_CURVE ( 'NONE', #12067, #7722, #8311, .T. ) ;
#7928 = CARTESIAN_POINT ( 'NONE',  ( -31.74999999999995026, 2.343373503921717580E-16, -3.499999999999996891 ) ) ;
#7929 = ADVANCED_FACE ( 'NONE', ( #2729 ), #519, .T. ) ;
#7930 = ORIENTED_EDGE ( 'NONE', *, *, #7773, .T. ) ;
#7931 = ORIENTED_EDGE ( 'NONE', *, *, #10834, .T. ) ;
#7932 = CARTESIAN_POINT ( 'NONE',  ( 0.000000000000000000, 5.483475578891600755, 3.488337222187588793 ) ) ;
#7933 = DIRECTION ( 'NONE',  ( 1.000000000000000000, 1.031065855027150586E-29, 2.218671295934092550E-30 ) ) ;
#7934 = CARTESIAN_POINT ( 'NONE',  ( 19.99999999999999645, 2.918117354836642363, 5.807029542149858337 ) ) ;
#7935 = DIRECTION ( 'NONE',  ( -1.000000000000000000, 1.010728034814421376E-30, 1.090846720500930387E-30 ) ) ;
#7936 = ORIENTED_EDGE ( 'NONE', *, *, #7611, .T. ) ;
#7937 = DIRECTION ( 'NONE',  ( 0.000000000000000000, 1.530455820933490821E-32, -1.000000000000000000 ) ) ;
#7938 = AXIS2_PLACEMENT_3D ( 'NONE', #3891, #9731, #9603 ) ;
#7939 = CARTESIAN_POINT ( 'NONE',  ( 40.00000000000000000, 39.34792583643766051, -14.91347054209568945 ) ) ;
#7940 = CIRCLE ( 'NONE', #8363, 7.400000000000009237 ) ;
#7941 = EDGE_CURVE ( 'NONE', #9038, #640, #11417, .T. ) ;
#7942 = CARTESIAN_POINT ( 'NONE',  ( 2.000000000000001776, -1.773042676681341856, 3.469446951953614189E-15 ) ) ;
#7943 = EDGE_LOOP ( 'NONE', ( #10992, #10528, #731, #11108 ) ) ;
#7944 = EDGE_LOOP ( 'NONE', ( #7655, #7950, #8681, #4377, #11265, #6741 ) ) ;
#7945 = CARTESIAN_POINT ( 'NONE',  ( 1.925929944387235853E-31, 4.618802153516985420, -3.504269196027888444 ) ) ;
#7946 = VERTEX_POINT ( 'NONE', #4645 ) ;
#7947 = ORIENTED_EDGE ( 'NONE', *, *, #3275, .T. ) ;
#7948 = PRODUCT_DEFINITION_FORMATION_WITH_SPECIFIED_SOURCE ( 'ANY', '', #10271, .NOT_KNOWN. ) ;
#7949 = CARTESIAN_POINT ( 'NONE',  ( 9.999999999999994671, 2.796709610837350812, 6.851161606081866751 ) ) ;
#7950 = ORIENTED_EDGE ( 'NONE', *, *, #5299, .T. ) ;
#7951 = AXIS2_PLACEMENT_3D ( 'NONE', #4719, #972, #6662 ) ;
#7952 = DIRECTION ( 'NONE',  ( 0.000000000000000000, 5.551115123125777772E-17, 1.000000000000000000 ) ) ;
#7953 = AXIS2_PLACEMENT_3D ( 'NONE', #4000, #4718, #8646 ) ;
#7954 = EDGE_CURVE ( 'NONE', #5440, #11959, #7538, .T. ) ;
#7955 = FACE_OUTER_BOUND ( 'NONE', #11683, .T. ) ;
#7956 = ORIENTED_EDGE ( 'NONE', *, *, #6765, .F. ) ;
#7957 = CARTESIAN_POINT ( 'NONE',  ( -11.83215956619923226, 30.00000000000000000, 1.999999999999999556 ) ) ;
#7958 = DIRECTION ( 'NONE',  ( 1.000000000000000000, -1.010728034814421376E-30, -1.090846720500930387E-30 ) ) ;
#7959 = VERTEX_POINT ( 'NONE', #1609 ) ;
#7960 = CIRCLE ( 'NONE', #11652, 6.499000000000008548 ) ;
#7961 = ORIENTED_EDGE ( 'NONE', *, *, #2971, .T. ) ;
#7962 = VERTEX_POINT ( 'NONE', #6516 ) ;
#7963 = EDGE_CURVE ( 'NONE', #2491, #9566, #5604, .T. ) ;
#7964 = FACE_OUTER_BOUND ( 'NONE', #1710, .T. ) ;
#7965 = DIRECTION ( 'NONE',  ( 0.000000000000000000, 0.000000000000000000, -1.000000000000000000 ) ) ;
#7966 = ORIENTED_EDGE ( 'NONE', *, *, #12552, .T. ) ;
#7967 = CARTESIAN_POINT ( 'NONE',  ( 19.99999999999999645, 1.764426149628130602, 7.186570834724196111 ) ) ;
#7968 = ORIENTED_EDGE ( 'NONE', *, *, #8229, .F. ) ;
#7969 = DIRECTION ( 'NONE',  ( 1.000000000000000000, 0.000000000000000000, 0.000000000000000000 ) ) ;
#7970 = EDGE_CURVE ( 'NONE', #2762, #10498, #7705, .T. ) ;
#7971 = ADVANCED_FACE ( 'NONE', ( #6647 ), #4451, .F. ) ;
#7972 = DIRECTION ( 'NONE',  ( 0.000000000000000000, 0.000000000000000000, 1.000000000000000000 ) ) ;
#7973 = DIRECTION ( 'NONE',  ( 0.000000000000000000, -5.551115123125776539E-17, -1.000000000000000000 ) ) ;
#7974 = EDGE_LOOP ( 'NONE', ( #3617, #12116, #1657, #10213 ) ) ;
#7975 = CARTESIAN_POINT ( 'NONE',  ( 19.99999999999999645, -2.171317488608541346, 7.074275960383707762 ) ) ;
#7976 = VERTEX_POINT ( 'NONE', #455 ) ;
#7977 = CARTESIAN_POINT ( 'NONE',  ( 0.000000000000000000, 6.321830586517925177, 1.817291089601352772 ) ) ;
#7978 = LINE ( 'NONE', #3814, #10494 ) ;
#7979 = CYLINDRICAL_SURFACE ( 'NONE', #11976, 2.800000000000003819 ) ;
#7980 = CYLINDRICAL_SURFACE ( 'NONE', #7306, 6.499000000000010324 ) ;
#7981 = ADVANCED_FACE ( 'NONE', ( #3623 ), #10553, .F. ) ;
#7982 = CARTESIAN_POINT ( 'NONE',  ( 19.99999999999997868, -0.9522442067290397549, -6.508557431545724192 ) ) ;
#7983 = CYLINDRICAL_SURFACE ( 'NONE', #11829, 2.800000000000003819 ) ;
#7984 = CARTESIAN_POINT ( 'NONE',  ( 0.000000000000000000, -3.178467454237179801, 5.758943784352561046 ) ) ;
#7985 = CARTESIAN_POINT ( 'NONE',  ( 0.000000000000000000, 0.000000000000000000, 0.000000000000000000 ) ) ;
#7986 = CARTESIAN_POINT ( 'NONE',  ( -40.00000000000000000, -19.99999999999999645, 2.000000000000003109 ) ) ;
#7987 = VECTOR ( 'NONE', #7035, 1000.000000000000000 ) ;
#7988 = AXIS2_PLACEMENT_3D ( 'NONE', #4241, #1528, #6433 ) ;
#7989 = VECTOR ( 'NONE', #10721, 999.9999999999998863 ) ;
#7990 = VERTEX_POINT ( 'NONE', #705 ) ;
#7991 = LINE ( 'NONE', #3127, #1487 ) ;
#7992 = DIRECTION ( 'NONE',  ( 1.000000000000000000, 1.031065855027150586E-29, -2.218671295934095703E-30 ) ) ;
#7993 = CARTESIAN_POINT ( 'NONE',  ( -3.999999999999993339, 1.700094919196852850, -3.320312364301083008 ) ) ;
#7994 = DIRECTION ( 'NONE',  ( -0.000000000000000000, 1.000000000000000000, -0.000000000000000000 ) ) ;
#7995 = ADVANCED_FACE ( 'NONE', ( #6581 ), #3437, .T. ) ;
#7996 = CARTESIAN_POINT ( 'NONE',  ( 0.000000000000000000, 0.000000000000000000, -0.3080913168122742518 ) ) ;
#7997 = VERTEX_POINT ( 'NONE', #3493 ) ;
#7998 = CARTESIAN_POINT ( 'NONE',  ( 2.000000000000001776, 1.773042676681338303, 0.000000000000000000 ) ) ;
#7999 = EDGE_CURVE ( 'NONE', #11730, #12228, #3800, .T. ) ;
#8000 = CIRCLE ( 'NONE', #9241, 7.400000000000009237 ) ;
#8001 = AXIS2_PLACEMENT_3D ( 'NONE', #6013, #1052, #4990 ) ;
#8002 = AXIS2_PLACEMENT_3D ( 'NONE', #7188, #5190, #1490 ) ;
#8003 = PLANE ( 'NONE',  #9348 ) ;
#8004 = DIRECTION ( 'NONE',  ( -1.000000000000000000, -5.916456789157575403E-31, 1.577021341797098793E-16 ) ) ;
#8005 = ORIENTED_EDGE ( 'NONE', *, *, #5620, .F. ) ;
#8006 = AXIS2_PLACEMENT_3D ( 'NONE', #422, #4350, #4670 ) ;
#8007 = ORIENTED_EDGE ( 'NONE', *, *, #5822, .F. ) ;
#8008 = EDGE_CURVE ( 'NONE', #12678, #1792, #2590, .T. ) ;
#8009 = CARTESIAN_POINT ( 'NONE',  ( -1.999999999999997335, 3.464101615137737067, -3.142992957459241676 ) ) ;
#8010 = EDGE_LOOP ( 'NONE', ( #11390, #12358, #11967, #3235 ) ) ;
#8011 = ORIENTED_EDGE ( 'NONE', *, *, #10607, .T. ) ;
#8012 = APPLICATION_PROTOCOL_DEFINITION ( 'draft international standard', 'automotive_design', 1998, #2144 ) ;
#8013 = CIRCLE ( 'NONE', #2479, 7.400000000000011902 ) ;
#8014 = DIRECTION ( 'NONE',  ( 0.000000000000000000, 0.000000000000000000, 1.000000000000000000 ) ) ;
#8015 = CIRCLE ( 'NONE', #3511, 2.800000000000004263 ) ;
#8016 = ORIENTED_EDGE ( 'NONE', *, *, #3893, .T. ) ;
#8017 = VECTOR ( 'NONE', #6715, 1000.000000000000114 ) ;
#8018 = CARTESIAN_POINT ( 'NONE',  ( -2.775557561562891351E-14, -4.618802153517012954, -0.5000000000000004441 ) ) ;
#8019 = DIRECTION ( 'NONE',  ( -1.000000000000000000, 1.010728034814421376E-30, 1.090846720500930387E-30 ) ) ;
#8020 = ORIENTED_EDGE ( 'NONE', *, *, #8128, .F. ) ;
#8021 = CARTESIAN_POINT ( 'NONE',  ( 0.000000000000000000, -1.268072931708452922, -6.374087545670245269 ) ) ;
#8022 = CARTESIAN_POINT ( 'NONE',  ( 9.999999999999998224, -12.99999999999999822, -6.123233995736765296E-16 ) ) ;
#8023 = DIRECTION ( 'NONE',  ( 0.000000000000000000, 0.5877852522924684742, 0.8090169943749506709 ) ) ;
#8024 = AXIS2_PLACEMENT_3D ( 'NONE', #11270, #7405, #3485 ) ;
#8025 = ORIENTED_EDGE ( 'NONE', *, *, #1262, .F. ) ;
#8026 = ORIENTED_EDGE ( 'NONE', *, *, #1801, .F. ) ;
#8027 = EDGE_LOOP ( 'NONE', ( #10789, #6099 ) ) ;
#8028 = ORIENTED_EDGE ( 'NONE', *, *, #3811, .T. ) ;
#8029 = DIRECTION ( 'NONE',  ( -1.000000000000000000, 1.010728034814421376E-30, 1.090846720500930387E-30 ) ) ;
#8030 = CARTESIAN_POINT ( 'NONE',  ( -4.175002511812136774, -2.208363329454923196, -3.469254087858258728 ) ) ;
#8031 = ORIENTED_EDGE ( 'NONE', *, *, #4954, .T. ) ;
#8032 = FACE_OUTER_BOUND ( 'NONE', #9210, .T. ) ;
#8033 = STYLED_ITEM ( 'NONE', ( #384 ), #10947 ) ;
#8034 = ORIENTED_EDGE ( 'NONE', *, *, #2074, .T. ) ;
#8035 = DIRECTION ( 'NONE',  ( -1.000000000000000000, 1.010728034814421376E-30, 1.090846720500930387E-30 ) ) ;
#8036 = CARTESIAN_POINT ( 'NONE',  ( 0.000000000000000000, 0.000000000000000000, 0.000000000000000000 ) ) ;
#8037 = CYLINDRICAL_SURFACE ( 'NONE', #7608, 2.500000000000003553 ) ;
#8038 = ORIENTED_EDGE ( 'NONE', *, *, #12324, .F. ) ;
#8040 = CARTESIAN_POINT ( 'NONE',  ( 33.61000000000001364, 0.000000000000000000, 0.000000000000000000 ) ) ;
#8039 = AXIS2_PLACEMENT_3D ( 'NONE', #1183, #8138, #7183 ) ;
#8041 = VERTEX_POINT ( 'NONE', #2531 ) ;
#8042 = CARTESIAN_POINT ( 'NONE',  ( -10.00000000000000178, 0.000000000000000000, 0.000000000000000000 ) ) ;
#8043 = ADVANCED_FACE ( 'NONE', ( #11476 ), #6452, .T. ) ;
#8044 = DIRECTION ( 'NONE',  ( 0.000000000000000000, 5.551115123125776539E-17, 1.000000000000000000 ) ) ;
#8045 = DIRECTION ( 'NONE',  ( 0.000000000000000000, 0.000000000000000000, -1.000000000000000000 ) ) ;
#8046 = CIRCLE ( 'NONE', #2104, 2.149999999999992362 ) ;
#8047 = CARTESIAN_POINT ( 'NONE',  ( -2.682243648011668480, -3.070208061305304437, -0.04852650426601311934 ) ) ;
#8048 = CARTESIAN_POINT ( 'NONE',  ( 34.00000000000000000, 1.610000000000000320, -1.734723475976807094E-14 ) ) ;
#8049 = DIRECTION ( 'NONE',  ( -2.243323199222248468E-30, 1.498801083243958569E-15, 1.000000000000000000 ) ) ;
#8050 = FACE_OUTER_BOUND ( 'NONE', #2390, .T. ) ;
#8051 = CARTESIAN_POINT ( 'NONE',  ( 0.000000000000000000, -3.612733913993642965, 6.458185013351672055 ) ) ;
#8052 = AXIS2_PLACEMENT_3D ( 'NONE', #4967, #9900, #70 ) ;
#8053 = ADVANCED_FACE ( 'NONE', ( #8566 ), #580, .F. ) ;
#8054 = VERTEX_POINT ( 'NONE', #8497 ) ;
#8055 = DIRECTION ( 'NONE',  ( -1.000000000000000000, 1.010728034814421376E-30, 1.090846720500930387E-30 ) ) ;
#8056 = DIRECTION ( 'NONE',  ( 0.000000000000000000, 0.000000000000000000, 1.000000000000000000 ) ) ;
#8057 = DIRECTION ( 'NONE',  ( 0.000000000000000000, 0.000000000000000000, 1.000000000000000000 ) ) ;
#8058 = DIRECTION ( 'NONE',  ( 0.000000000000000000, 0.8660254037844392627, 0.4999999999999990008 ) ) ;
#8059 = DIRECTION ( 'NONE',  ( 0.000000000000000000, -0.8345732537213078617, 0.5508969814520944253 ) ) ;
#8060 = ORIENTED_EDGE ( 'NONE', *, *, #10919, .T. ) ;
#8061 = AXIS2_PLACEMENT_3D ( 'NONE', #8447, #1492, #8577 ) ;
#8062 = CARTESIAN_POINT ( 'NONE',  ( 0.000000000000000000, 0.000000000000000000, 0.000000000000000000 ) ) ;
#8063 = AXIS2_PLACEMENT_3D ( 'NONE', #4105, #8029, #3164 ) ;
#8064 = CYLINDRICAL_SURFACE ( 'NONE', #88, 7.400000000000010125 ) ;
#8065 = SURFACE_SIDE_STYLE ('',( #10774 ) ) ;
#8066 = EDGE_CURVE ( 'NONE', #9690, #11825, #12445, .T. ) ;
#8067 = EDGE_LOOP ( 'NONE', ( #2180, #2926 ) ) ;
#8068 = DIRECTION ( 'NONE',  ( -1.000000000000000000, 1.010728034814421376E-30, 1.090846720500930387E-30 ) ) ;
#8069 = VERTEX_POINT ( 'NONE', #3679 ) ;
#8070 = AXIS2_PLACEMENT_3D ( 'NONE', #2168, #355, #10128 ) ;
#8071 = ORIENTED_EDGE ( 'NONE', *, *, #8073, .T. ) ;
#8072 = PRODUCT_CONTEXT ( 'NONE', #12271, 'mechanical' ) ;
#8073 = EDGE_CURVE ( 'NONE', #276, #4606, #6475, .T. ) ;
#8074 = CIRCLE ( 'NONE', #2545, 2.800000000000002487 ) ;
#8075 = AXIS2_PLACEMENT_3D ( 'NONE', #9555, #3661, #9364 ) ;
#8076 = EDGE_CURVE ( 'NONE', #6900, #2828, #4769, .T. ) ;
#8077 = CARTESIAN_POINT ( 'NONE',  ( 19.99999999999999645, 0.000000000000000000, 0.000000000000000000 ) ) ;
#8078 = ORIENTED_EDGE ( 'NONE', *, *, #3040, .T. ) ;
#8079 = LINE ( 'NONE', #10249, #9417 ) ;
#8080 = CYLINDRICAL_SURFACE ( 'NONE', #4386, 6.499000000000010324 ) ;
#8081 = ORIENTED_EDGE ( 'NONE', *, *, #3389, .F. ) ;
#8082 = FACE_OUTER_BOUND ( 'NONE', #5950, .T. ) ;
#8083 = DIRECTION ( 'NONE',  ( -1.000000000000000000, 1.010728034814421376E-30, 1.090846720500930387E-30 ) ) ;
#8084 = EDGE_CURVE ( 'NONE', #11206, #8600, #6697, .T. ) ;
#8085 = CARTESIAN_POINT ( 'NONE',  ( 0.1750025118121487089, 4.719839900820611334, -3.469254087858254731 ) ) ;
#8086 = VECTOR ( 'NONE', #9540, 1000.000000000000000 ) ;
#8087 = ORIENTED_EDGE ( 'NONE', *, *, #3622, .T. ) ;
#8088 = EDGE_LOOP ( 'NONE', ( #3228, #9164, #7334 ) ) ;
#8089 = VERTEX_POINT ( 'NONE', #6767 ) ;
#8090 = ORIENTED_EDGE ( 'NONE', *, *, #12719, .T. ) ;
#8091 = ADVANCED_FACE ( 'NONE', ( #10806 ), #3045, .T. ) ;
#8092 = CYLINDRICAL_SURFACE ( 'NONE', #9096, 7.400000000000010125 ) ;
#8093 = ADVANCED_FACE ( 'NONE', ( #8695 ), #3002, .T. ) ;
#8094 = CARTESIAN_POINT ( 'NONE',  ( 40.00000000000000711, 18.52447679111068268, -16.77732469694377926 ) ) ;
#8095 = VERTEX_POINT ( 'NONE', #11598 ) ;
#8096 = DIRECTION ( 'NONE',  ( 0.000000000000000000, 0.000000000000000000, 1.000000000000000000 ) ) ;
#8097 = ORIENTED_EDGE ( 'NONE', *, *, #10599, .T. ) ;
#8098 = FACE_OUTER_BOUND ( 'NONE', #3536, .T. ) ;
#8099 = CIRCLE ( 'NONE', #12443, 4.499999999999999112 ) ;
#8100 = CARTESIAN_POINT ( 'NONE',  ( 40.00000000000000711, 18.52447679111068268, -16.77732469694377926 ) ) ;
#8101 = CARTESIAN_POINT ( 'NONE',  ( 14.00000000000000000, 53.63999999999999346, -5.000000000000001776 ) ) ;
#8102 = ORIENTED_EDGE ( 'NONE', *, *, #754, .F. ) ;
#8103 = DIRECTION ( 'NONE',  ( 0.000000000000000000, 0.000000000000000000, -1.000000000000000000 ) ) ;
#8104 = ORIENTED_EDGE ( 'NONE', *, *, #1285, .T. ) ;
#8105 = LINE ( 'NONE', #2454, #3956 ) ;
#8106 = AXIS2_PLACEMENT_3D ( 'NONE', #973, #8888, #2071 ) ;
#8107 = CIRCLE ( 'NONE', #5039, 14.99999999999998934 ) ;
#8108 = EDGE_CURVE ( 'NONE', #8996, #11904, #11020, .T. ) ;
#8109 = DIRECTION ( 'NONE',  ( 0.5000000000000022204, 0.8660254037844374864, 0.000000000000000000 ) ) ;
#8110 = DIRECTION ( 'NONE',  ( 0.000000000000000000, 0.000000000000000000, -1.000000000000000000 ) ) ;
#8111 = EDGE_CURVE ( 'NONE', #11957, #4395, #7908, .T. ) ;
#8112 = PRODUCT_DEFINITION_SHAPE ( 'NONE', 'NONE',  #10818 ) ;
#8113 = DIRECTION ( 'NONE',  ( -1.454462294001239290E-30, 0.7227948638273881121, 0.6910626489868684219 ) ) ;
#8114 = DIRECTION ( 'NONE',  ( 0.000000000000000000, -5.551115123125775923E-17, -1.000000000000000000 ) ) ;
#8115 = CIRCLE ( 'NONE', #8535, 4.000000000000000000 ) ;
#8116 = CARTESIAN_POINT ( 'NONE',  ( 20.00000000000000000, 39.34792583643766051, -19.21347054209566707 ) ) ;
#8117 = CARTESIAN_POINT ( 'NONE',  ( 14.00000000000000000, 30.00000000000000000, -4.000000000000000000 ) ) ;
#8118 = FACE_OUTER_BOUND ( 'NONE', #6358, .T. ) ;
#8119 = SURFACE_STYLE_FILL_AREA ( #4134 ) ;
#8120 = EDGE_CURVE ( 'NONE', #7484, #803, #9754, .T. ) ;
#8121 = ORIENTED_EDGE ( 'NONE', *, *, #8761, .T. ) ;
#8122 = CIRCLE ( 'NONE', #12055, 4.000000000000001776 ) ;
#8123 = DIRECTION ( 'NONE',  ( -1.000000000000000000, 1.010728034814421376E-30, 1.090846720500930387E-30 ) ) ;
#8124 = FACE_OUTER_BOUND ( 'NONE', #2774, .T. ) ;
#8125 = CARTESIAN_POINT ( 'NONE',  ( 19.99999999999999645, 0.000000000000000000, 0.000000000000000000 ) ) ;
#8126 = DIRECTION ( 'NONE',  ( -1.000000000000000000, 1.010728034814421376E-30, 1.090846720500930387E-30 ) ) ;
#8127 = ORIENTED_EDGE ( 'NONE', *, *, #10446, .T. ) ;
#8128 = EDGE_CURVE ( 'NONE', #2092, #3887, #10618, .T. ) ;
#8129 = FACE_OUTER_BOUND ( 'NONE', #3259, .T. ) ;
#8130 = EDGE_CURVE ( 'NONE', #156, #7571, #719, .T. ) ;
#8131 = EDGE_CURVE ( 'NONE', #529, #10905, #8115, .T. ) ;
#8132 = CARTESIAN_POINT ( 'NONE',  ( 0.000000000000000000, 0.000000000000000000, 0.000000000000000000 ) ) ;
#8133 = EDGE_CURVE ( 'NONE', #11698, #9285, #4830, .T. ) ;
#8134 = SURFACE_SIDE_STYLE ('',( #5303 ) ) ;
#8135 = AXIS2_PLACEMENT_3D ( 'NONE', #7476, #11413, #7354 ) ;
#8136 = VERTEX_POINT ( 'NONE', #1986 ) ;
#8137 = AXIS2_PLACEMENT_3D ( 'NONE', #2315, #3232, #7965 ) ;
#8138 = DIRECTION ( 'NONE',  ( 1.000000000000000000, -1.010728034814421376E-30, -1.090846720500930387E-30 ) ) ;
#8139 = ORIENTED_EDGE ( 'NONE', *, *, #11842, .F. ) ;
#8140 = ORIENTED_EDGE ( 'NONE', *, *, #46, .F. ) ;
#8141 = CONTEXT_DEPENDENT_SHAPE_REPRESENTATION ( #4851, #1621 ) ;
#8142 = DIRECTION ( 'NONE',  ( -0.000000000000000000, -1.000000000000000000, -0.000000000000000000 ) ) ;
#8143 = ORIENTED_EDGE ( 'NONE', *, *, #8846, .T. ) ;
#8144 =( NAMED_UNIT ( * ) PLANE_ANGLE_UNIT ( ) SI_UNIT ( $, .RADIAN. ) );
#8145 = FACE_OUTER_BOUND ( 'NONE', #7595, .T. ) ;
#8146 = VERTEX_POINT ( 'NONE', #8813 ) ;
#8147 = FILL_AREA_STYLE ('',( #10985 ) ) ;
#8148 = DIRECTION ( 'NONE',  ( -1.000000000000000000, 1.010728034814421376E-30, 1.090846720500930387E-30 ) ) ;
#8149 = VECTOR ( 'NONE', #1576, 1000.000000000000000 ) ;
#8150 = CARTESIAN_POINT ( 'NONE',  ( 27.00000000000001421, 70.57443853988016258, -5.364737079370081041 ) ) ;
#8151 = CARTESIAN_POINT ( 'NONE',  ( 20.00000000000000000, 8.163911011730665024, -17.95311239921186441 ) ) ;
#8152 = EDGE_CURVE ( 'NONE', #1263, #3837, #512, .T. ) ;
#8153 = ORIENTED_EDGE ( 'NONE', *, *, #2261, .F. ) ;
#8154 = ORIENTED_EDGE ( 'NONE', *, *, #5398, .T. ) ;
#8155 = ORIENTED_EDGE ( 'NONE', *, *, #8553, .F. ) ;
#8156 = ORIENTED_EDGE ( 'NONE', *, *, #11926, .T. ) ;
#8157 = AXIS2_PLACEMENT_3D ( 'NONE', #11361, #12331, #2544 ) ;
#8158 = CARTESIAN_POINT ( 'NONE',  ( 27.00000000000001421, 39.34792583643766761, -17.06347054209568270 ) ) ;
#8159 = ADVANCED_FACE ( 'NONE', ( #5916 ), #3987, .F. ) ;
#8160 = CIRCLE ( 'NONE', #11864, 2.000000000000000888 ) ;
#8161 = ADVANCED_FACE ( 'NONE', ( #7852 ), #3129, .F. ) ;
#8162 = CARTESIAN_POINT ( 'NONE',  ( -2.756197834950048442, -3.027510591568753462, -3.223146290110009193 ) ) ;
#8163 = ORIENTED_EDGE ( 'NONE', *, *, #12001, .F. ) ;
#8164 = DIRECTION ( 'NONE',  ( 0.000000000000000000, -0.2951046417778627751, -0.9554649393887560960 ) ) ;
#8165 = ORIENTED_EDGE ( 'NONE', *, *, #8553, .T. ) ;
#8166 = DIRECTION ( 'NONE',  ( -1.000000000000000000, 1.010728034814421376E-30, 1.090846720500930387E-30 ) ) ;
#8167 = CIRCLE ( 'NONE', #8823, 6.499000000000008548 ) ;
#8168 = CIRCLE ( 'NONE', #2633, 2.800000000000002931 ) ;
#8169 = EDGE_CURVE ( 'NONE', #955, #568, #8320, .T. ) ;
#8170 = VECTOR ( 'NONE', #9465, 1000.000000000000000 ) ;
#8171 = CARTESIAN_POINT ( 'NONE',  ( 19.99999999999999645, -4.907279493584762342, 4.380262188593320616 ) ) ;
#8172 = EDGE_CURVE ( 'NONE', #1206, #5403, #2056, .T. ) ;
#8173 = B_SPLINE_CURVE_WITH_KNOTS ( 'NONE', 3,
 ( #1496, #655, #4597, #10174, #5427, #9341, #4465, #2414 ),
 .UNSPECIFIED., .F., .F.,
 ( 4, 2, 2, 4 ),
 ( 0.000000000000000000, 0.002450665683189816660, 0.003675998524784724990, 0.004901331366379633320 ),
 .UNSPECIFIED. ) ;
#8174 = CARTESIAN_POINT ( 'NONE',  ( 14.00000000000000000, 44.64000000000000057, -6.938893903907228378E-15 ) ) ;
#8175 = VERTEX_POINT ( 'NONE', #2125 ) ;
#8176 = CARTESIAN_POINT ( 'NONE',  ( 0.000000000000000000, -6.453973581750240385, 0.7636923504068595658 ) ) ;
#8177 = ORIENTED_EDGE ( 'NONE', *, *, #2919, .T. ) ;
#8178 = DIRECTION ( 'NONE',  ( 1.133987551255203069E-30, -0.9909497617679331460, -0.1342332658176667304 ) ) ;
#8179 = AXIS2_PLACEMENT_3D ( 'NONE', #3667, #3729, #11396 ) ;
#8180 = PLANE ( 'NONE',  #3512 ) ;
#8181 = CARTESIAN_POINT ( 'NONE',  ( 19.99999999999997868, 6.321830586517925177, 1.817291089601345888 ) ) ;
#8182 = DIRECTION ( 'NONE',  ( 0.000000000000000000, 0.000000000000000000, 1.000000000000000000 ) ) ;
#8183 = CARTESIAN_POINT ( 'NONE',  ( -11.83215956619923226, 30.00000000000000000, -2.000000000000000888 ) ) ;
#8184 = CARTESIAN_POINT ( 'NONE',  ( -11.83215956619923226, 30.00000000000000000, -2.000000000000000888 ) ) ;
#8185 = DIRECTION ( 'NONE',  ( -1.000000000000000000, 1.010728034814421376E-30, 1.090846720500930387E-30 ) ) ;
#8186 = FACE_OUTER_BOUND ( 'NONE', #4154, .T. ) ;
#8187 = EDGE_CURVE ( 'NONE', #7946, #6318, #3210, .T. ) ;
#8188 = SURFACE_STYLE_FILL_AREA ( #3380 ) ;
#8189 = ORIENTED_EDGE ( 'NONE', *, *, #11467, .F. ) ;
#8190 = CARTESIAN_POINT ( 'NONE',  ( 19.99999999999999645, 7.164568425986781897, -1.851744925564387856 ) ) ;
#8191 = CARTESIAN_POINT ( 'NONE',  ( 19.99999999999997868, 5.483475578891663815, -3.488337222187519515 ) ) ;
#8192 = CIRCLE ( 'NONE', #6971, 0.2000000000000000944 ) ;
#8193 = CARTESIAN_POINT ( 'NONE',  ( -4.197477534772225738, 0.8522413273724327443, -3.505042416683237683 ) ) ;
#8194 = CARTESIAN_POINT ( 'NONE',  ( 2.000000000000001776, 1.773042676681341856, -3.469446951953614189E-15 ) ) ;
#8195 = LINE ( 'NONE', #3329, #12261 ) ;
#8196 = CARTESIAN_POINT ( 'NONE',  ( 0.000000000000000000, 2.918117354836644139, 5.807029542149858337 ) ) ;
#8197 = DIRECTION ( 'NONE',  ( 1.000000000000000000, -1.010728034814421376E-30, -1.090846720500930387E-30 ) ) ;
#8198 = VECTOR ( 'NONE', #10872, 1000.000000000000000 ) ;
#8199 = VECTOR ( 'NONE', #3038, 1000.000000000000000 ) ;
#8200 = ORIENTED_EDGE ( 'NONE', *, *, #11234, .T. ) ;
#8201 = CARTESIAN_POINT ( 'NONE',  ( -10.00000000000000178, 0.000000000000000000, 0.000000000000000000 ) ) ;
#8202 = ORIENTED_EDGE ( 'NONE', *, *, #2814, .T. ) ;
#8203 = AXIS2_PLACEMENT_3D ( 'NONE', #12367, #5645, #11583 ) ;
#8204 = VERTEX_POINT ( 'NONE', #4305 ) ;
#8205 = ITEM_DEFINED_TRANSFORMATION ( 'NONE', 'NONE', #10425,  #12422 ) ;
#8206 = EDGE_CURVE ( 'NONE', #11576, #3412, #5245, .T. ) ;
#8207 = ADVANCED_FACE ( 'NONE', ( #12111 ), #1085, .T. ) ;
#8208 = ORIENTED_EDGE ( 'NONE', *, *, #5909, .T. ) ;
#8209 = DIRECTION ( 'NONE',  ( -1.000000000000000000, 1.010728034814421376E-30, 1.090846720500930387E-30 ) ) ;
#8210 = DIRECTION ( 'NONE',  ( -1.140150527077241873E-30, 0.000000000000000000, 1.000000000000000000 ) ) ;
#8211 = CONICAL_SURFACE ( 'NONE', #2682, 5.560781378645573980, 1.221730476396046816 ) ;
#8212 = CIRCLE ( 'NONE', #906, 2.800000000000004263 ) ;
#8213 = DIRECTION ( 'NONE',  ( 1.140150527077241873E-30, 0.000000000000000000, -1.000000000000000000 ) ) ;
#8214 = CARTESIAN_POINT ( 'NONE',  ( 19.99999999999999645, -6.213893036447818652, 1.903820982021499297 ) ) ;
#8215 = VECTOR ( 'NONE', #10310, 1000.000000000000000 ) ;
#8216 = DIRECTION ( 'NONE',  ( 0.000000000000000000, 1.000000000000000000, 0.000000000000000000 ) ) ;
#8217 = CARTESIAN_POINT ( 'NONE',  ( -2.712762565639325718, 3.052587955997613456, -3.430618716626822717 ) ) ;
#8218 = CIRCLE ( 'NONE', #2686, 0.2000000000000000944 ) ;
#8219 = DIRECTION ( 'NONE',  ( 6.902532920683844539E-31, -0.9749279121818259508, 0.2225209339563041233 ) ) ;
#8220 = ORIENTED_EDGE ( 'NONE', *, *, #1914, .T. ) ;
#8221 = ORIENTED_EDGE ( 'NONE', *, *, #342, .T. ) ;
#8222 = ORIENTED_EDGE ( 'NONE', *, *, #1164, .T. ) ;
#8223 = VECTOR ( 'NONE', #3107, 1000.000000000000114 ) ;
#8224 = ORIENTED_EDGE ( 'NONE', *, *, #5018, .F. ) ;
#8225 = AXIS2_PLACEMENT_3D ( 'NONE', #7235, #2274, #6255 ) ;
#8226 = CIRCLE ( 'NONE', #7404, 7.999999999999998224 ) ;
#8227 = CARTESIAN_POINT ( 'NONE',  ( 3.469446951953614189E-14, -3.469446951953614189E-15, -4.974600000000009459 ) ) ;
#8228 = PRODUCT_DEFINITION_SHAPE ( 'NONE', 'NONE',  #5164 ) ;
#8229 = EDGE_CURVE ( 'NONE', #2119, #2228, #7912, .T. ) ;
#8230 = DIRECTION ( 'NONE',  ( -1.000000000000000000, 0.000000000000000000, 0.000000000000000000 ) ) ;
#8231 = VERTEX_POINT ( 'NONE', #5213 ) ;
#8232 = DIRECTION ( 'NONE',  ( 0.000000000000000000, 0.000000000000000000, 1.000000000000000000 ) ) ;
#8233 = EDGE_LOOP ( 'NONE', ( #4215, #960, #2358, #10780 ) ) ;
#8234 = CARTESIAN_POINT ( 'NONE',  ( 9.999999999999994671, -0.8732627748488634989, 7.348293143721422283 ) ) ;
#8235 = DIRECTION ( 'NONE',  ( -1.000000000000000000, 1.010728034814421376E-30, 1.090846720500930387E-30 ) ) ;
#8236 = VECTOR ( 'NONE', #8300, 1000.000000000000000 ) ;
#8237 = AXIS2_PLACEMENT_3D ( 'NONE', #4491, #7512, #11448 ) ;
#8238 = DIRECTION ( 'NONE',  ( -1.000000000000000000, 1.010728034814421376E-30, 1.090846720500930387E-30 ) ) ;
#8239 = CARTESIAN_POINT ( 'NONE',  ( 11.00000000000001599, -12.50000000000000178, 5.000000000000007994 ) ) ;
#8240 = ORIENTED_EDGE ( 'NONE', *, *, #5572, .F. ) ;
#8241 = ORIENTED_EDGE ( 'NONE', *, *, #10237, .T. ) ;
#8242 = EDGE_CURVE ( 'NONE', #4356, #2884, #2584, .T. ) ;
#8243 = CARTESIAN_POINT ( 'NONE',  ( 40.00000000000000711, 8.611173066148738897, -18.09125363591105540 ) ) ;
#8244 = PRESENTATION_LAYER_ASSIGNMENT (  '', '', ( #4122 ) ) ;
#8245 = FILL_AREA_STYLE_COLOUR ( '', #10700 ) ;
#8246 = EDGE_CURVE ( 'NONE', #8622, #837, #10158, .T. ) ;
#8247 = FACE_OUTER_BOUND ( 'NONE', #1604, .T. ) ;
#8248 = EDGE_CURVE ( 'NONE', #11074, #2378, #7718, .T. ) ;
#8249 = PLANE ( 'NONE',  #12390 ) ;
#8250 = DIRECTION ( 'NONE',  ( 0.000000000000000000, 0.000000000000000000, 1.000000000000000000 ) ) ;
#8251 = EDGE_CURVE ( 'NONE', #10664, #927, #12457, .T. ) ;
#8252 = CARTESIAN_POINT ( 'NONE',  ( 2.000000000000001776, -1.773042676681341856, 3.469446951953614189E-15 ) ) ;
#8253 = CARTESIAN_POINT ( 'NONE',  ( 14.00000000000000000, 44.64000000000000057, -4.000000000000007105 ) ) ;
#8254 = ORIENTED_EDGE ( 'NONE', *, *, #12483, .F. ) ;
#8255 = DIRECTION ( 'NONE',  ( 0.000000000000000000, -0.5128992774058948045, -0.8584487936018729837 ) ) ;
#8256 = CARTESIAN_POINT ( 'NONE',  ( 11.00000000000002665, 12.50000000000000000, 5.000000000000004441 ) ) ;
#8257 = AXIS2_PLACEMENT_3D ( 'NONE', #11366, #2548, #10379 ) ;
#8258 = ORIENTED_EDGE ( 'NONE', *, *, #345, .T. ) ;
#8259 = DIRECTION ( 'NONE',  ( 0.000000000000000000, 0.000000000000000000, 1.000000000000000000 ) ) ;
#8260 = DIRECTION ( 'NONE',  ( -1.000000000000000000, -5.916456789157575403E-31, 1.577021341797099039E-16 ) ) ;
#8261 = FACE_OUTER_BOUND ( 'NONE', #12309, .T. ) ;
#8262 = CARTESIAN_POINT ( 'NONE',  ( -10.00000000000000178, 0.000000000000000000, 0.000000000000000000 ) ) ;
#8263 = DIRECTION ( 'NONE',  ( 0.000000000000000000, -1.000000000000000000, 0.000000000000000000 ) ) ;
#8264 = DIRECTION ( 'NONE',  ( 0.000000000000000000, -0.7227948638273978821, 0.6910626489868579858 ) ) ;
#8265 = TOROIDAL_SURFACE ( 'NONE', #7249, 8.000000000000000000, 4.000000000000000000 ) ;
#8266 = ORIENTED_EDGE ( 'NONE', *, *, #11757, .T. ) ;
#8267 = DIRECTION ( 'NONE',  ( 0.000000000000000000, 4.478906847412192569E-32, -1.000000000000000000 ) ) ;
#8268 = ORIENTED_EDGE ( 'NONE', *, *, #4910, .F. ) ;
#8269 = ORIENTED_EDGE ( 'NONE', *, *, #4784, .F. ) ;
#8270 = CONTEXT_DEPENDENT_SHAPE_REPRESENTATION ( #9852, #9526 ) ;
#8271 = VERTEX_POINT ( 'NONE', #11007 ) ;
#8272 = CLOSED_SHELL ( 'NONE', ( #8370, #2516, #9460, #9435, #11302, #3444, #660, #11843, #4383, #7896, #769, #7855, #141, #7299, #1353, #8528, #11965, #1339, #6044, #6918, #7971, #12363, #10674, #8598, #11137, #12433, #2413 ) ) ;
#8273 = ADVANCED_FACE ( 'NONE', ( #2190 ), #10147, .F. ) ;
#8274 = DIRECTION ( 'NONE',  ( 0.000000000000000000, 0.000000000000000000, 1.000000000000000000 ) ) ;
#8275 = AXIS2_PLACEMENT_3D ( 'NONE', #6118, #3933, #3993 ) ;
#8276 = DIRECTION ( 'NONE',  ( -1.000000000000000000, 0.000000000000000000, 0.000000000000000000 ) ) ;
#8277 = DIRECTION ( 'NONE',  ( -8.073498326871282186E-31, -0.2660368455666824450, 0.9639628606958512425 ) ) ;
#8278 = CARTESIAN_POINT ( 'NONE',  ( 19.99999999999997868, -3.612733913993553703, -6.458185013351741333 ) ) ;
#8279 = VERTEX_POINT ( 'NONE', #5153 ) ;
#8280 = CARTESIAN_POINT ( 'NONE',  ( -1.257172072275692054, 3.892973519170934260, -3.433252694550601447 ) ) ;
#8281 = DIRECTION ( 'NONE',  ( -1.000000000000000000, -2.206481006425900381E-16, 8.674603474570138454E-17 ) ) ;
#8282 = ORIENTED_EDGE ( 'NONE', *, *, #7208, .T. ) ;
#8283 = ORIENTED_EDGE ( 'NONE', *, *, #10112, .T. ) ;
#8284 = AXIS2_PLACEMENT_3D ( 'NONE', #4461, #5556, #9463 ) ;
#8285 = ORIENTED_EDGE ( 'NONE', *, *, #9531, .T. ) ;
#8286 = AXIS2_PLACEMENT_3D ( 'NONE', #7723, #6758, #7470 ) ;
#8287 = ORIENTED_EDGE ( 'NONE', *, *, #9614, .F. ) ;
#8288 = CARTESIAN_POINT ( 'NONE',  ( 0.000000000000000000, -4.046291478462172186, -5.186098161460352074 ) ) ;
#8289 =( NAMED_UNIT ( * ) SI_UNIT ( $, .STERADIAN. ) SOLID_ANGLE_UNIT ( ) );
#8290 = ORIENTED_EDGE ( 'NONE', *, *, #1500, .T. ) ;
#8291 = CARTESIAN_POINT ( 'NONE',  ( -17.00000000000002842, 19.99999999999998579, 9.850000000000036948 ) ) ;
#8292 = ORIENTED_EDGE ( 'NONE', *, *, #12324, .T. ) ;
#8293 = AXIS2_PLACEMENT_3D ( 'NONE', #5002, #7063, #9167 ) ;
#8294 = DIRECTION ( 'NONE',  ( 1.000000000000000000, 0.000000000000000000, 0.000000000000000000 ) ) ;
#8295 = CARTESIAN_POINT ( 'NONE',  ( 0.000000000000000000, -6.484265599627184073, 1.105616797298897280 ) ) ;
#8296 = EDGE_CURVE ( 'NONE', #8271, #5523, #3807, .T. ) ;
#8297 = DIRECTION ( 'NONE',  ( 0.000000000000000000, 0.8805955318567392220, -0.4738686624729965824 ) ) ;
#8298 = EDGE_CURVE ( 'NONE', #1836, #640, #11002, .T. ) ;
#8299 = ADVANCED_FACE ( 'NONE', ( #2323 ), #1340, .T. ) ;
#8300 = DIRECTION ( 'NONE',  ( -1.848892746611746419E-31, -1.000000000000000000, 3.250006781153460502E-32 ) ) ;
#8301 = VERTEX_POINT ( 'NONE', #7280 ) ;
#8302 = CIRCLE ( 'NONE', #2779, 2.100000000000000089 ) ;
#8303 = ORIENTED_EDGE ( 'NONE', *, *, #5623, .F. ) ;
#8304 = CARTESIAN_POINT ( 'NONE',  ( 11.00000000000003020, -30.00000000000000000, 25.00000000000007105 ) ) ;
#8305 = SHAPE_REPRESENTATION ( 'cover 1', ( #12422 ), #6859 ) ;
#8306 =( NAMED_UNIT ( * ) PLANE_ANGLE_UNIT ( ) SI_UNIT ( $, .RADIAN. ) );
#8307 = CARTESIAN_POINT ( 'NONE',  ( 4.000000000000000000, 2.309401076758487381, -4.999999999999984013 ) ) ;
#8308 = DIRECTION ( 'NONE',  ( -1.000000000000000000, 0.000000000000000000, 0.000000000000000000 ) ) ;
#8309 = AXIS2_PLACEMENT_3D ( 'NONE', #5147, #12049, #6043 ) ;
#8310 = CARTESIAN_POINT ( 'NONE',  ( 19.99999999999999645, -6.884685972239648066, -2.713134545806132003 ) ) ;
#8311 = LINE ( 'NONE', #10293, #6894 ) ;
#8312 = CARTESIAN_POINT ( 'NONE',  ( 0.000000000000000000, -6.969736844459714753, 2.486517307195110327 ) ) ;
#8313 = VERTEX_POINT ( 'NONE', #9194 ) ;
#8314 = LINE ( 'NONE', #9147, #4315 ) ;
#8315 = VECTOR ( 'NONE', #3513, 1000.000000000000000 ) ;
#8316 = DIRECTION ( 'NONE',  ( -1.848892746611746419E-31, -1.000000000000000000, 3.250006781153460502E-32 ) ) ;
#8317 = EDGE_CURVE ( 'NONE', #742, #6542, #10577, .T. ) ;
#8318 = ORIENTED_EDGE ( 'NONE', *, *, #7466, .T. ) ;
#8319 = CARTESIAN_POINT ( 'NONE',  ( 2.000000000000001776, 0.000000000000000000, 0.000000000000000000 ) ) ;
#8321 = DIRECTION ( 'NONE',  ( -1.000000000000000000, 1.010728034814421376E-30, 1.090846720500930387E-30 ) ) ;
#8320 = CIRCLE ( 'NONE', #5038, 2.800000000000003819 ) ;
#8322 = CARTESIAN_POINT ( 'NONE',  ( 33.00000000000001421, 81.84122341717352356, -27.68198508464163510 ) ) ;
#8323 = AXIS2_PLACEMENT_3D ( 'NONE', #8295, #12239, #3423 ) ;
#8324 = DIRECTION ( 'NONE',  ( 0.000000000000000000, -1.530455820933490821E-32, 1.000000000000000000 ) ) ;
#8325 = EDGE_CURVE ( 'NONE', #3019, #3594, #6487, .T. ) ;
#8326 = DIRECTION ( 'NONE',  ( 1.140150527077240122E-30, -1.776356839400250465E-15, -1.000000000000000000 ) ) ;
#8327 = EDGE_CURVE ( 'NONE', #3589, #6992, #5861, .T. ) ;
#8328 = PRODUCT ( 'socket head cap screw_iso_ISO 4762 M4 x 25 - 25N', 'socket head cap screw_iso_ISO 4762 M4 x 25 - 25N', '', ( #5063 ) ) ;
#8329 = LINE ( 'NONE', #3516, #7195 ) ;
#8330 = ORIENTED_EDGE ( 'NONE', *, *, #6449, .F. ) ;
#8331 = DIRECTION ( 'NONE',  ( 1.154721252774410375E-34, 3.250006781153453386E-32, -1.000000000000000000 ) ) ;
#8332 = EDGE_LOOP ( 'NONE', ( #12019, #5380, #5626, #10399 ) ) ;
#8333 = VECTOR ( 'NONE', #9374, 1000.000000000000114 ) ;
#8334 = VERTEX_POINT ( 'NONE', #2388 ) ;
#8335 = CIRCLE ( 'NONE', #9144, 4.999999999999999112 ) ;
#8336 = ORIENTED_EDGE ( 'NONE', *, *, #4106, .F. ) ;
#8337 = ORIENTED_EDGE ( 'NONE', *, *, #5499, .T. ) ;
#8338 = CARTESIAN_POINT ( 'NONE',  ( -10.00000000000000178, 0.000000000000000000, 0.000000000000000000 ) ) ;
#8339 = SURFACE_SIDE_STYLE ('',( #11244 ) ) ;
#8340 = CYLINDRICAL_SURFACE ( 'NONE', #816, 6.000000000000000000 ) ;
#8341 = CARTESIAN_POINT ( 'NONE',  ( 2.000000000000001776, 1.773042676681338303, 0.000000000000000000 ) ) ;
#8342 = ORIENTED_EDGE ( 'NONE', *, *, #11702, .F. ) ;
#8343 = DIRECTION ( 'NONE',  ( 0.000000000000000000, 5.551115123125777772E-17, 1.000000000000000000 ) ) ;
#8344 = EDGE_CURVE ( 'NONE', #2170, #12673, #1533, .T. ) ;
#8345 = AXIS2_PLACEMENT_3D ( 'NONE', #1113, #7937, #4801 ) ;
#8346 = FACE_OUTER_BOUND ( 'NONE', #4916, .T. ) ;
#8347 = ORIENTED_EDGE ( 'NONE', *, *, #2637, .T. ) ;
#8348 = VERTEX_POINT ( 'NONE', #9436 ) ;
#8349 = ORIENTED_EDGE ( 'NONE', *, *, #5148, .T. ) ;
#8350 = ORIENTED_EDGE ( 'NONE', *, *, #5219, .T. ) ;
#8351 = CARTESIAN_POINT ( 'NONE',  ( 9.999999999999998224, 30.00000000000000000, -6.123233995736765296E-16 ) ) ;
#8352 = EDGE_CURVE ( 'NONE', #9071, #2762, #6439, .T. ) ;
#8353 = CARTESIAN_POINT ( 'NONE',  ( 50.00005079999998969, 5.510332127717259942E-15, -2.500000000000010658 ) ) ;
#8354 = VERTEX_POINT ( 'NONE', #8424 ) ;
#8355 = COLOUR_RGB ( '', 0.40784314, 0.44705882, 0.49803922) ;
#8356 = DIRECTION ( 'NONE',  ( -1.000000000000000000, 0.000000000000000000, 1.159061634649218351E-16 ) ) ;
#8357 = ORIENTED_EDGE ( 'NONE', *, *, #8745, .F. ) ;
#8358 = CARTESIAN_POINT ( 'NONE',  ( 19.99999999999999645, -5.610543508060415796, -3.433640984893324699 ) ) ;
#8359 = CARTESIAN_POINT ( 'NONE',  ( 27.00000000000001421, 81.84122341717352356, -27.68198508464163510 ) ) ;
#8360 = FACE_OUTER_BOUND ( 'NONE', #9539, .T. ) ;
#8361 = AXIS2_PLACEMENT_3D ( 'NONE', #10049, #1044, #4074 ) ;
#8362 = CARTESIAN_POINT ( 'NONE',  ( 19.99999999999999645, -6.182645281642477286, -2.245659411033190445 ) ) ;
#8363 = AXIS2_PLACEMENT_3D ( 'NONE', #7379, #11566, #2692 ) ;
#8364 = ORIENTED_EDGE ( 'NONE', *, *, #269, .F. ) ;
#8365 = VERTEX_POINT ( 'NONE', #1404 ) ;
#8366 = DIRECTION ( 'NONE',  ( -1.000000000000000000, 1.010728034814421376E-30, 1.090846720500930387E-30 ) ) ;
#8367 = EDGE_CURVE ( 'NONE', #7959, #7387, #7509, .T. ) ;
#8368 = FACE_OUTER_BOUND ( 'NONE', #12193, .T. ) ;
#8369 = AXIS2_PLACEMENT_3D ( 'NONE', #3797, #7725, #11471 ) ;
#8370 = ADVANCED_FACE ( 'NONE', ( #1469 ), #106, .F. ) ;
#8371 = AXIS2_PLACEMENT_3D ( 'NONE', #9716, #4843, #8826 ) ;
#8372 = CARTESIAN_POINT ( 'NONE',  ( -35.00000000000006395, 19.99999999999999645, 2.168404344971058172E-15 ) ) ;
#8373 = CIRCLE ( 'NONE', #10000, 6.000000000000000000 ) ;
#8374 = CARTESIAN_POINT ( 'NONE',  ( 4.197478902586993854, -0.8524102783748621626, -3.505063281295508038 ) ) ;
#8375 = CARTESIAN_POINT ( 'NONE',  ( 19.99999999999997868, -1.966014849756994254, -6.277170897746295886 ) ) ;
#8376 = LINE ( 'NONE', #3558, #9425 ) ;
#8377 = EDGE_LOOP ( 'NONE', ( #2507, #2918, #9239, #3413 ) ) ;
#8378 = SHAPE_REPRESENTATION ( 'fixed position lower roller', ( #12422 ), #7225 ) ;
#8379 = CARTESIAN_POINT ( 'NONE',  ( -11.83215956619923226, 30.00000000000000000, -2.000000000000000888 ) ) ;
#8380 = AXIS2_PLACEMENT_3D ( 'NONE', #880, #9879, #6751 ) ;
#8381 = CARTESIAN_POINT ( 'NONE',  ( 19.99999999999999645, -6.413745496774120092, 3.691052519622234129 ) ) ;
#8382 = DIRECTION ( 'NONE',  ( -1.000000000000000000, 1.010728034814421376E-30, 1.090846720500930387E-30 ) ) ;
#8383 = EDGE_CURVE ( 'NONE', #11905, #8539, #9143, .T. ) ;
#8384 = ORIENTED_EDGE ( 'NONE', *, *, #445, .T. ) ;
#8385 = DIRECTION ( 'NONE',  ( 0.000000000000000000, 0.000000000000000000, 1.000000000000000000 ) ) ;
#8386 = CARTESIAN_POINT ( 'NONE',  ( 19.99999999999997868, 6.718789039999997215, -3.101269713516725091 ) ) ;
#8387 = LINE ( 'NONE', #534, #8170 ) ;
#8388 = CARTESIAN_POINT ( 'NONE',  ( 19.99999999999999645, 5.483475578891613189, 3.488337222187588793 ) ) ;
#8389 = CARTESIAN_POINT ( 'NONE',  ( -15.00000000000003375, 19.99999999999998579, 9.850000000000033396 ) ) ;
#8390 = CARTESIAN_POINT ( 'NONE',  ( 19.99999999999999645, -4.621065432155107011, 4.569765340993028779 ) ) ;
#8391 = CARTESIAN_POINT ( 'NONE',  ( 0.000000000000000000, -3.612733913993552815, -6.458185013351741333 ) ) ;
#8392 = DIRECTION ( 'NONE',  ( -1.848892746611746419E-31, -1.000000000000000000, -3.250006781153453386E-32 ) ) ;
#8393 = EDGE_LOOP ( 'NONE', ( #5, #6757, #3579, #7904 ) ) ;
#8394 = AXIS2_PLACEMENT_3D ( 'NONE', #10456, #5510, #12411 ) ;
#8395 = ORIENTED_EDGE ( 'NONE', *, *, #11408, .T. ) ;
#8396 = ADVANCED_FACE ( 'NONE', ( #8360 ), #5044, .T. ) ;
#8397 = ORIENTED_EDGE ( 'NONE', *, *, #3515, .F. ) ;
#8398 = DIRECTION ( 'NONE',  ( 0.000000000000000000, 0.000000000000000000, 1.000000000000000000 ) ) ;
#8399 = EDGE_CURVE ( 'NONE', #10778, #10168, #4571, .T. ) ;
#8400 = DIRECTION ( 'NONE',  ( 0.000000000000000000, -0.2951046417778627751, -0.9554649393887560960 ) ) ;
#8401 = DIRECTION ( 'NONE',  ( 0.000000000000000000, 0.000000000000000000, -1.000000000000000000 ) ) ;
#8402 = DIRECTION ( 'NONE',  ( 0.000000000000000000, 0.3513748240813435175, -0.9362348706397368714 ) ) ;
#8403 = ORIENTED_EDGE ( 'NONE', *, *, #4914, .T. ) ;
#8404 = DIRECTION ( 'NONE',  ( -1.000000000000000000, -1.031065855027150586E-29, 2.218671295934095703E-30 ) ) ;
#8405 = EDGE_CURVE ( 'NONE', #1045, #499, #5530, .T. ) ;
#8406 = AXIS2_PLACEMENT_3D ( 'NONE', #5901, #7772, #4811 ) ;
#8407 = CARTESIAN_POINT ( 'NONE',  ( 19.99999999999997868, 6.018220532833812975, -2.453165835849195453 ) ) ;
#8408 = ORIENTED_EDGE ( 'NONE', *, *, #12398, .F. ) ;
#8409 = ORIENTED_EDGE ( 'NONE', *, *, #4335, .F. ) ;
#8410 = DIRECTION ( 'NONE',  ( 6.938893903907224680E-17, -3.250006781153453386E-32, 1.000000000000000000 ) ) ;
#8411 = ORIENTED_EDGE ( 'NONE', *, *, #4317, .T. ) ;
#8412 = ORIENTED_EDGE ( 'NONE', *, *, #2971, .F. ) ;
#8413 = DIRECTION ( 'NONE',  ( 0.000000000000000000, 0.000000000000000000, -1.000000000000000000 ) ) ;
#8414 = VECTOR ( 'NONE', #9206, 1000.000000000000000 ) ;
#8415 = SURFACE_STYLE_USAGE ( .BOTH. , #433 ) ;
#8416 = PRESENTATION_LAYER_ASSIGNMENT (  '', '', ( #12336 ) ) ;
#8417 = ORIENTED_EDGE ( 'NONE', *, *, #7176, .T. ) ;
#8418 = CARTESIAN_POINT ( 'NONE',  ( 0.000000000000000000, 3.019282868015085164, 6.756029230465983026 ) ) ;
#8419 = CARTESIAN_POINT ( 'NONE',  ( 14.00000000000000000, 30.00000000000000000, 0.000000000000000000 ) ) ;
#8420 = COLOUR_RGB ( '', 0.09019608, 0.27058824, 0.51372549) ;
#8421 = ORIENTED_EDGE ( 'NONE', *, *, #3183, .F. ) ;
#8422 = DIRECTION ( 'NONE',  ( 1.000000000000000000, -1.010728034814421376E-30, -1.090846720500930387E-30 ) ) ;
#8423 = DIRECTION ( 'NONE',  ( 0.000000000000000000, 0.000000000000000000, -1.000000000000000000 ) ) ;
#8424 = CARTESIAN_POINT ( 'NONE',  ( 19.99999999999997868, 5.025702764809158118, -5.431603052487340655 ) ) ;
#8425 = AXIS2_PLACEMENT_3D ( 'NONE', #12051, #378, #4307 ) ;
#8426 = VECTOR ( 'NONE', #10953, 1000.000000000000000 ) ;
#8427 = AXIS2_PLACEMENT_3D ( 'NONE', #5898, #6746, #998 ) ;
#8428 = CARTESIAN_POINT ( 'NONE',  ( 19.99999999999997868, 6.146182963951668299, 2.112211157443887100 ) ) ;
#8429 = ORIENTED_EDGE ( 'NONE', *, *, #7602, .F. ) ;
#8430 = ORIENTED_EDGE ( 'NONE', *, *, #11372, .F. ) ;
#8431 = FACE_OUTER_BOUND ( 'NONE', #1823, .T. ) ;
#8432 = DIRECTION ( 'NONE',  ( 1.000000000000000000, -0.000000000000000000, -0.000000000000000000 ) ) ;
#8433 = CIRCLE ( 'NONE', #6386, 24.99999999999998934 ) ;
#8434 = AXIS2_PLACEMENT_3D ( 'NONE', #584, #709, #4518 ) ;
#8435 = AXIS2_PLACEMENT_3D ( 'NONE', #6246, #10154, #1346 ) ;
#8436 = DIRECTION ( 'NONE',  ( -1.140150527077241873E-30, 0.000000000000000000, 1.000000000000000000 ) ) ;
#8437 = DIRECTION ( 'NONE',  ( 0.000000000000000000, 0.000000000000000000, 1.000000000000000000 ) ) ;
#8438 = DIRECTION ( 'NONE',  ( -1.000000000000000000, 1.010728034814421376E-30, 1.090846720500930387E-30 ) ) ;
#8439 = EDGE_CURVE ( 'NONE', #4775, #11591, #9254, .T. ) ;
#8440 = ORIENTED_EDGE ( 'NONE', *, *, #5762, .F. ) ;
#8441 = DIRECTION ( 'NONE',  ( -3.266377185680748504E-31, 0.8805955318567392220, -0.4738686624729964159 ) ) ;
#8442 = AXIS2_PLACEMENT_3D ( 'NONE', #3652, #1897, #9607 ) ;
#8443 = CARTESIAN_POINT ( 'NONE',  ( 19.99999999999999645, 5.280167904461726458, 3.922743398397384063 ) ) ;
#8444 =( NAMED_UNIT ( * ) PLANE_ANGLE_UNIT ( ) SI_UNIT ( $, .RADIAN. ) );
#8445 = DIRECTION ( 'NONE',  ( 0.000000000000000000, 1.000000000000000000, 0.000000000000000000 ) ) ;
#8446 = ORIENTED_EDGE ( 'NONE', *, *, #9108, .T. ) ;
#8447 = CARTESIAN_POINT ( 'NONE',  ( 19.99999999999999645, 0.000000000000000000, 0.000000000000000000 ) ) ;
#8448 = LINE ( 'NONE', #3447, #8909 ) ;
#8449 = CYLINDRICAL_SURFACE ( 'NONE', #9586, 7.400000000000010125 ) ;
#8450 = CARTESIAN_POINT ( 'NONE',  ( 4.000000000000019540, -2.309401076758522464, -3.433295621305367806 ) ) ;
#8451 = DIRECTION ( 'NONE',  ( -1.000000000000000000, -1.081682119347366197E-16, 6.938893903907228378E-17 ) ) ;
#8452 = CYLINDRICAL_SURFACE ( 'NONE', #12023, 2.800000000000003819 ) ;
#8453 = EDGE_CURVE ( 'NONE', #8729, #6857, #11462, .T. ) ;
#8454 = EDGE_CURVE ( 'NONE', #7962, #12032, #10590, .T. ) ;
#8455 = CARTESIAN_POINT ( 'NONE',  ( -5.560781378645554440, -2.788447640341961550E-15, -4.000000000000010658 ) ) ;
#8456 = CARTESIAN_POINT ( 'NONE',  ( 28.99999999999999645, 3.469446951953614189E-15, 0.000000000000000000 ) ) ;
#8457 = ORIENTED_EDGE ( 'NONE', *, *, #3565, .T. ) ;
#8458 = VERTEX_POINT ( 'NONE', #5399 ) ;
#8459 = VERTEX_POINT ( 'NONE', #2449 ) ;
#8460 = DIRECTION ( 'NONE',  ( 1.000000000000000000, -1.010728034814421376E-30, -1.090846720500930387E-30 ) ) ;
#8461 = SURFACE_SIDE_STYLE ('',( #4548 ) ) ;
#8462 = DIRECTION ( 'NONE',  ( -1.000000000000000000, 1.006188713385347367E-17, 3.844790828812615713E-17 ) ) ;
#8463 = AXIS2_PLACEMENT_3D ( 'NONE', #7742, #8766, #9839 ) ;
#8464 = FACE_OUTER_BOUND ( 'NONE', #9633, .T. ) ;
#8465 = ORIENTED_EDGE ( 'NONE', *, *, #603, .T. ) ;
#8466 = PLANE ( 'NONE',  #4010 ) ;
#8467 = DIRECTION ( 'NONE',  ( -1.000000000000000000, -1.848892746611742259E-31, 1.154721252774410589E-34 ) ) ;
#8468 = VERTEX_POINT ( 'NONE', #6565 ) ;
#8469 = ORIENTED_EDGE ( 'NONE', *, *, #696, .T. ) ;
#8470 = DIRECTION ( 'NONE',  ( 2.218671295934093250E-30, -5.551115123125776539E-17, -1.000000000000000000 ) ) ;
#8471 = ORIENTED_EDGE ( 'NONE', *, *, #8868, .T. ) ;
#8472 = ORIENTED_EDGE ( 'NONE', *, *, #11707, .T. ) ;
#8473 = AXIS2_PLACEMENT_3D ( 'NONE', #3873, #9965, #5029 ) ;
#8474 =( NAMED_UNIT ( * ) PLANE_ANGLE_UNIT ( ) SI_UNIT ( $, .RADIAN. ) );
#8475 = ORIENTED_EDGE ( 'NONE', *, *, #8827, .T. ) ;
#8476 = DIRECTION ( 'NONE',  ( 0.000000000000000000, 0.2660368455666689003, 0.9639628606958551282 ) ) ;
#8477 = EDGE_CURVE ( 'NONE', #7420, #6820, #2176, .T. ) ;
#8478 = DIRECTION ( 'NONE',  ( 0.000000000000000000, -0.1785568947986227173, -0.9839295885986321100 ) ) ;
#8479 = ORIENTED_EDGE ( 'NONE', *, *, #11241, .F. ) ;
#8480 = CYLINDRICAL_SURFACE ( 'NONE', #541, 2.800000000000003819 ) ;
#8481 = CARTESIAN_POINT ( 'NONE',  ( 0.1999999999999987899, 1.831867990631508193E-16, 3.300000000000003375 ) ) ;
#8482 = CIRCLE ( 'NONE', #8284, 2.800000000000004263 ) ;
#8483 = CARTESIAN_POINT ( 'NONE',  ( 9.999999999999998224, -2.171317488608444535, -7.074275960383742401 ) ) ;
#8484 = AXIS2_PLACEMENT_3D ( 'NONE', #12040, #5261, #431 ) ;
#8485 = ADVANCED_FACE ( 'NONE', ( #10282 ), #10479, .T. ) ;
#8486 = DIRECTION ( 'NONE',  ( -1.000000000000000000, 1.010728034814421376E-30, 1.090846720500930387E-30 ) ) ;
#8487 = ADVANCED_FACE ( 'NONE', ( #1666 ), #5593, .T. ) ;
#8488 = EDGE_LOOP ( 'NONE', ( #2145, #4607, #5123, #1310 ) ) ;
#8489 = ORIENTED_EDGE ( 'NONE', *, *, #872, .T. ) ;
#8490 = CARTESIAN_POINT ( 'NONE',  ( 0.000000000000000000, 0.000000000000000000, 0.000000000000000000 ) ) ;
#8491 = AXIS2_PLACEMENT_3D ( 'NONE', #6479, #1447, #5375 ) ;
#8492 = DIRECTION ( 'NONE',  ( -1.000000000000000222, -2.891205793294676847E-16, -1.942890293094023946E-16 ) ) ;
#8493 = ORIENTED_EDGE ( 'NONE', *, *, #4942, .F. ) ;
#8494 = DIRECTION ( 'NONE',  ( 5.208075316782974243E-17, 0.1525077710325581370, 0.9883022714608525883 ) ) ;
#8495 = AXIS2_PLACEMENT_3D ( 'NONE', #4494, #6495, #9424 ) ;
#8496 = FACE_OUTER_BOUND ( 'NONE', #12428, .T. ) ;
#8497 = CARTESIAN_POINT ( 'NONE',  ( 19.99999999999999645, 2.180689217871860652, 6.122221454264574092 ) ) ;
#8498 = CIRCLE ( 'NONE', #10752, 2.800000000000002931 ) ;
#8499 = CARTESIAN_POINT ( 'NONE',  ( 6.000000000000000000, 49.63999999999998636, -7.000000000000000888 ) ) ;
#8500 = EDGE_LOOP ( 'NONE', ( #2854, #6476, #7316, #1714 ) ) ;
#8501 = PLANE ( 'NONE',  #11102 ) ;
#8502 = CARTESIAN_POINT ( 'NONE',  ( 9.999999999999998224, -0.8732627748487576946, -7.348293143721449816 ) ) ;
#8503 = EDGE_CURVE ( 'NONE', #3286, #6138, #10211, .T. ) ;
#8504 = ADVANCED_FACE ( 'NONE', ( #5948, #987 ), #8787, .F. ) ;
#8505 = DIRECTION ( 'NONE',  ( 0.000000000000000000, 0.2660368455666689003, 0.9639628606958551282 ) ) ;
#8506 = CIRCLE ( 'NONE', #5839, 6.499000000000006771 ) ;
#8507 = EDGE_LOOP ( 'NONE', ( #9350, #698, #6756, #5648 ) ) ;
#8508 = CARTESIAN_POINT ( 'NONE',  ( 33.00000000000001421, 48.04086878529346194, 39.26975893117280947 ) ) ;
#8509 = CARTESIAN_POINT ( 'NONE',  ( 19.99999999999999645, 0.000000000000000000, 0.000000000000000000 ) ) ;
#8510 = CYLINDRICAL_SURFACE ( 'NONE', #12497, 7.400000000000010125 ) ;
#8511 = DIRECTION ( 'NONE',  ( 1.140150527077241873E-30, 0.000000000000000000, -1.000000000000000000 ) ) ;
#8512 = LINE ( 'NONE', #12461, #4646 ) ;
#8513 = CIRCLE ( 'NONE', #4817, 2.800000000000003819 ) ;
#8514 = CARTESIAN_POINT ( 'NONE',  ( 6.000000000000000000, 49.63999999999998636, -19.00000000000000355 ) ) ;
#8515 = LINE ( 'NONE', #10697, #10880 ) ;
#8516 = UNCERTAINTY_MEASURE_WITH_UNIT (LENGTH_MEASURE( 1.000000000000000082E-05 ), #5432, 'distance_accuracy_value', 'NONE');
#8517 = EDGE_CURVE ( 'NONE', #12737, #8539, #7724, .T. ) ;
#8518 = CARTESIAN_POINT ( 'NONE',  ( -3.999999999999963585, -2.309401076758515359, -3.433295621305398893 ) ) ;
#8519 = ORIENTED_EDGE ( 'NONE', *, *, #7230, .F. ) ;
#8520 = AXIS2_PLACEMENT_3D ( 'NONE', #8048, #136, #1165 ) ;
#8521 = ORIENTED_EDGE ( 'NONE', *, *, #3132, .F. ) ;
#8522 = VECTOR ( 'NONE', #4691, 1000.000000000000000 ) ;
#8523 = ORIENTED_EDGE ( 'NONE', *, *, #8692, .T. ) ;
#8524 = EDGE_CURVE ( 'NONE', #7997, #2985, #11527, .T. ) ;
#8525 = CARTESIAN_POINT ( 'NONE',  ( 19.99999999999997868, 6.496448636052932990, 0.1820882179769736653 ) ) ;
#8526 = FACE_OUTER_BOUND ( 'NONE', #6270, .T. ) ;
#8528 = ADVANCED_FACE ( 'NONE', ( #10840 ), #8003, .F. ) ;
#8527 = LINE ( 'NONE', #3647, #4908 ) ;
#8529 = DIRECTION ( 'NONE',  ( 0.000000000000000000, 0.000000000000000000, 1.000000000000000000 ) ) ;
#8530 = VERTEX_POINT ( 'NONE', #3071 ) ;
#8531 = EDGE_CURVE ( 'NONE', #3047, #8975, #5462, .T. ) ;
#8532 = CYLINDRICAL_SURFACE ( 'NONE', #7914, 6.499000000000010324 ) ;
#8533 = FACE_OUTER_BOUND ( 'NONE', #2423, .T. ) ;
#8534 = ORIENTED_EDGE ( 'NONE', *, *, #132, .T. ) ;
#8535 = AXIS2_PLACEMENT_3D ( 'NONE', #770, #4702, #10678 ) ;
#8536 = VERTEX_POINT ( 'NONE', #11951 ) ;
#8537 = LINE ( 'NONE', #10715, #2248 ) ;
#8538 = ORIENTED_EDGE ( 'NONE', *, *, #2189, .F. ) ;
#8539 = VERTEX_POINT ( 'NONE', #5115 ) ;
#8540 = PRODUCT_DEFINITION_SHAPE ( 'NONE', 'NONE',  #12251 ) ;
#8541 = ORIENTED_EDGE ( 'NONE', *, *, #11482, .F. ) ;
#8542 = DIRECTION ( 'NONE',  ( 1.000000000000000000, 1.081682119347366321E-16, -5.551115123125780237E-17 ) ) ;
#8543 = DIRECTION ( 'NONE',  ( -1.417484439069003136E-30, 0.9195277725514489076, 0.3930250316539277144 ) ) ;
#8544 = ORIENTED_EDGE ( 'NONE', *, *, #2030, .T. ) ;
#8545 = EDGE_CURVE ( 'NONE', #9347, #1577, #8749, .T. ) ;
#8546 = AXIS2_PLACEMENT_3D ( 'NONE', #9027, #4336, #3388 ) ;
#8547 = CYLINDRICAL_SURFACE ( 'NONE', #3462, 19.99999999999999645 ) ;
#8548 = CARTESIAN_POINT ( 'NONE',  ( -45.00000000000013500, 30.00000000000000000, 2.000000000000007994 ) ) ;
#8549 = CARTESIAN_POINT ( 'NONE',  ( 0.000000000000000000, 1.395418990828293460, -6.428133065596405515 ) ) ;
#8550 = UNCERTAINTY_MEASURE_WITH_UNIT (LENGTH_MEASURE( 1.000000000000000082E-05 ), #9200, 'distance_accuracy_value', 'NONE');
#8551 = EDGE_CURVE ( 'NONE', #5403, #4493, #7697, .T. ) ;
#8552 = ORIENTED_EDGE ( 'NONE', *, *, #4760, .T. ) ;
#8553 = EDGE_CURVE ( 'NONE', #11062, #5702, #10709, .T. ) ;
#8554 = ORIENTED_EDGE ( 'NONE', *, *, #62, .F. ) ;
#8555 =( REPRESENTATION_RELATIONSHIP ('NONE','NONE', #10018, #11514 ) REPRESENTATION_RELATIONSHIP_WITH_TRANSFORMATION ( #4476 )SHAPE_REPRESENTATION_RELATIONSHIP( ) );
#8556 = CARTESIAN_POINT ( 'NONE',  ( -18.00000000000000355, 29.99999999999998224, 3.000000000000008438 ) ) ;
#8557 = VECTOR ( 'NONE', #453, 1000.000000000000000 ) ;
#8558 = DIRECTION ( 'NONE',  ( -3.658689512969242901E-17, -2.891205793294675368E-16, 1.000000000000000000 ) ) ;
#8559 = VERTEX_POINT ( 'NONE', #5823 ) ;
#8560 = DIRECTION ( 'NONE',  ( -1.000000000000000000, 1.010728034814421376E-30, 1.090846720500930387E-30 ) ) ;
#8561 = EDGE_CURVE ( 'NONE', #1053, #9867, #494, .T. ) ;
#8562 = CARTESIAN_POINT ( 'NONE',  ( -17.00000000000000000, 30.00000000000000000, 3.000000000000030198 ) ) ;
#8563 = ADVANCED_FACE ( 'NONE', ( #6012 ), #153, .F. ) ;
#8564 = CIRCLE ( 'NONE', #332, 6.499000000000009436 ) ;
#8565 = VECTOR ( 'NONE', #859, 1000.000000000000000 ) ;
#8566 = FACE_OUTER_BOUND ( 'NONE', #9319, .T. ) ;
#8567 = CYLINDRICAL_SURFACE ( 'NONE', #2040, 6.499000000000010324 ) ;
#8568 = EDGE_CURVE ( 'NONE', #11904, #10248, #91, .T. ) ;
#8569 = VERTEX_POINT ( 'NONE', #6076 ) ;
#8570 = CARTESIAN_POINT ( 'NONE',  ( 14.00000000000000000, 30.00000000000000000, 6.000000000000000000 ) ) ;
#8571 = VERTEX_POINT ( 'NONE', #5055 ) ;
#8572 = LINE ( 'NONE', #12513, #5389 ) ;
#8573 = AXIS2_PLACEMENT_3D ( 'NONE', #9269, #4131, #329 ) ;
#8574 = AXIS2_PLACEMENT_3D ( 'NONE', #214, #5051, #2287 ) ;
#8575 = CIRCLE ( 'NONE', #7151, 2.499999999999992006 ) ;
#8576 = CARTESIAN_POINT ( 'NONE',  ( 0.000000000000000000, 0.4528593230175778639, -7.386130139224209579 ) ) ;
#8577 = DIRECTION ( 'NONE',  ( 0.000000000000000000, 0.000000000000000000, 1.000000000000000000 ) ) ;
#8578 = CARTESIAN_POINT ( 'NONE',  ( -9.860132971832690885, 30.00000000000000000, -1.666666666666667629 ) ) ;
#8579 = DIRECTION ( 'NONE',  ( -1.000000000000000000, -5.916456789157575403E-31, -2.465190328815656418E-32 ) ) ;
#8580 = CYLINDRICAL_SURFACE ( 'NONE', #3451, 6.999999999999999112 ) ;
#8581 = CARTESIAN_POINT ( 'NONE',  ( 2.886521338340684917, 0.000000000000000000, 0.000000000000000000 ) ) ;
#8582 = DIRECTION ( 'NONE',  ( 1.000000000000000000, 0.000000000000000000, -1.159061634649218351E-16 ) ) ;
#8583 = CIRCLE ( 'NONE', #8991, 1.535500000000000087 ) ;
#8584 = PLANE ( 'NONE',  #5747 ) ;
#8585 = DIRECTION ( 'NONE',  ( -1.000000000000000000, 1.010728034814421376E-30, 1.090846720500930387E-30 ) ) ;
#8586 = VERTEX_POINT ( 'NONE', #7879 ) ;
#8587 = VERTEX_POINT ( 'NONE', #31 ) ;
#8588 = ORIENTED_EDGE ( 'NONE', *, *, #4351, .F. ) ;
#8589 = CARTESIAN_POINT ( 'NONE',  ( 40.00000000000000711, 18.52447679111068268, -16.77732469694377926 ) ) ;
#8590 = DIRECTION ( 'NONE',  ( 0.000000000000000000, 1.000000000000000000, 0.000000000000000000 ) ) ;
#8591 = CARTESIAN_POINT ( 'NONE',  ( 6.000000000000000000, 49.63999999999998636, -7.000000000000000888 ) ) ;
#8592 = DIRECTION ( 'NONE',  ( 1.000000000000000000, -6.162975822039154730E-33, -4.563833282352349791E-17 ) ) ;
#8593 = ORIENTED_EDGE ( 'NONE', *, *, #5283, .F. ) ;
#8594 = CARTESIAN_POINT ( 'NONE',  ( 4.000000000000000000, 2.309401076758487381, -4.999999999999984013 ) ) ;
#8595 = DIRECTION ( 'NONE',  ( 0.000000000000000000, 0.000000000000000000, 1.000000000000000000 ) ) ;
#8596 = ORIENTED_EDGE ( 'NONE', *, *, #11784, .T. ) ;
#8597 = ORIENTED_EDGE ( 'NONE', *, *, #8614, .T. ) ;
#8598 = ADVANCED_FACE ( 'NONE', ( #9797 ), #9925, .F. ) ;
#8599 = CARTESIAN_POINT ( 'NONE',  ( 19.99999999999999645, -4.357840574720623472, 4.821434073521965402 ) ) ;
#8600 = VERTEX_POINT ( 'NONE', #3898 ) ;
#8601 = AXIS2_PLACEMENT_3D ( 'NONE', #9635, #5726, #1737 ) ;
#8602 = ADVANCED_FACE ( 'NONE', ( #7825 ), #11758, .T. ) ;
#8603 = ORIENTED_EDGE ( 'NONE', *, *, #12134, .F. ) ;
#8604 = PRESENTATION_STYLE_ASSIGNMENT (( #4751 ) ) ;
#8605 = DIRECTION ( 'NONE',  ( 0.000000000000000000, 0.000000000000000000, 1.000000000000000000 ) ) ;
#8606 = ORIENTED_EDGE ( 'NONE', *, *, #8845, .F. ) ;
#8607 = CARTESIAN_POINT ( 'NONE',  ( 0.000000000000000000, 0.000000000000000000, 0.000000000000000000 ) ) ;
#8608 = FACE_OUTER_BOUND ( 'NONE', #6554, .T. ) ;
#8609 = ORIENTED_EDGE ( 'NONE', *, *, #2000, .F. ) ;
#8610 = CARTESIAN_POINT ( 'NONE',  ( 20.00000000000000000, 9.597108420813796670, -18.39576936187866352 ) ) ;
#8611 = CARTESIAN_POINT ( 'NONE',  ( 19.99999999999999645, 0.000000000000000000, 0.000000000000000000 ) ) ;
#8612 = AXIS2_PLACEMENT_3D ( 'NONE', #1527, #750, #10598 ) ;
#8613 = VERTEX_POINT ( 'NONE', #4018 ) ;
#8614 = EDGE_CURVE ( 'NONE', #10850, #6306, #1115, .T. ) ;
#8615 = AXIS2_PLACEMENT_3D ( 'NONE', #9610, #6682, #7829 ) ;
#8616 = AXIS2_PLACEMENT_3D ( 'NONE', #9695, #5978, #11657 ) ;
#8617 = PRODUCT_RELATED_PRODUCT_CATEGORY ( 'part', '', ( #5241 ) ) ;
#8618 = ORIENTED_EDGE ( 'NONE', *, *, #2758, .F. ) ;
#8619 = CYLINDRICAL_SURFACE ( 'NONE', #8286, 6.499000000000010324 ) ;
#8620 = AXIS2_PLACEMENT_3D ( 'NONE', #3277, #7190, #2300 ) ;
#8621 = DIRECTION ( 'NONE',  ( -1.000000000000000222, -1.081682119347366444E-16, 0.000000000000000000 ) ) ;
#8622 = VERTEX_POINT ( 'NONE', #9157 ) ;
#8623 = DIRECTION ( 'NONE',  ( -3.437775699846489820E-17, -0.2951046417778627751, -0.9554649393887560960 ) ) ;
#8624 = CARTESIAN_POINT ( 'NONE',  ( 11.00000000000003020, 30.00000000000000000, -9.742497179615118866E-31 ) ) ;
#8625 = AXIS2_PLACEMENT_3D ( 'NONE', #5805, #10950, #17 ) ;
#8626 = AXIS2_PLACEMENT_3D ( 'NONE', #5746, #1759, #5681 ) ;
#8627 = AXIS2_PLACEMENT_3D ( 'NONE', #11112, #3022, #5064 ) ;
#8628 = CARTESIAN_POINT ( 'NONE',  ( 1.243802165048784492, -3.900692638707469850, -3.223146290109814682 ) ) ;
#8629 = VECTOR ( 'NONE', #4735, 1000.000000000000000 ) ;
#8630 = EDGE_CURVE ( 'NONE', #7387, #7959, #503, .T. ) ;
#8631 = DIRECTION ( 'NONE',  ( -1.000000000000000000, 0.000000000000000000, 0.000000000000000000 ) ) ;
#8632 = ORIENTED_EDGE ( 'NONE', *, *, #5621, .F. ) ;
#8633 = LINE ( 'NONE', #2796, #610 ) ;
#8634 = ORIENTED_EDGE ( 'NONE', *, *, #2669, .F. ) ;
#8635 = ADVANCED_FACE ( 'NONE', ( #12076 ), #11103, .T. ) ;
#8636 = LINE ( 'NONE', #5795, #3138 ) ;
#8637 = EDGE_CURVE ( 'NONE', #490, #11957, #6885, .T. ) ;
#8638 = TOROIDAL_SURFACE ( 'NONE', #2052, 2.200000000000001066, 0.2000000000000000111 ) ;
#8640 = AXIS2_PLACEMENT_3D ( 'NONE', #8379, #3440, #10224 ) ;
#8639 =( NAMED_UNIT ( * ) PLANE_ANGLE_UNIT ( ) SI_UNIT ( $, .RADIAN. ) );
#8641 = AXIS2_PLACEMENT_3D ( 'NONE', #1158, #11147, #9138 ) ;
#8642 = DIRECTION ( 'NONE',  ( 1.503766100577551477E-30, -0.6579387259397028176, -0.7530714660036194052 ) ) ;
#8643 = DIRECTION ( 'NONE',  ( 0.000000000000000000, -0.9997704357740726522, -0.02142605311579142205 ) ) ;
#8644 = EDGE_CURVE ( 'NONE', #5144, #5654, #1736, .T. ) ;
#8645 = DIRECTION ( 'NONE',  ( -1.000000000000000000, 1.010728034814421376E-30, 1.090846720500930387E-30 ) ) ;
#8646 = DIRECTION ( 'NONE',  ( 0.000000000000000000, 0.000000000000000000, 1.000000000000000000 ) ) ;
#8647 = FACE_OUTER_BOUND ( 'NONE', #4739, .T. ) ;
#8648 = DIRECTION ( 'NONE',  ( 1.224646799147352714E-16, 1.177425296209236909E-30, 1.000000000000000000 ) ) ;
#8649 = AXIS2_PLACEMENT_3D ( 'NONE', #10134, #9174, #9237 ) ;
#8650 = VECTOR ( 'NONE', #5208, 1000.000000000000000 ) ;
#8651 = CARTESIAN_POINT ( 'NONE',  ( 2.344047193898584958, 3.265465875126461803, 6.475990398232750876E-15 ) ) ;
#8652 = SURFACE_SIDE_STYLE ('',( #9533 ) ) ;
#8653 = UNCERTAINTY_MEASURE_WITH_UNIT (LENGTH_MEASURE( 1.000000000000000082E-05 ), #280, 'distance_accuracy_value', 'NONE');
#8654 = CARTESIAN_POINT ( 'NONE',  ( 19.99999999999999645, -5.932103089875941038, 2.654647609586679113 ) ) ;
#8656 = ORIENTED_EDGE ( 'NONE', *, *, #9775, .T. ) ;
#8655 = ADVANCED_FACE ( 'NONE', ( #2290 ), #8064, .T. ) ;
#8657 = VERTEX_POINT ( 'NONE', #9097 ) ;
#8658 = VERTEX_POINT ( 'NONE', #3390 ) ;
#8659 = CARTESIAN_POINT ( 'NONE',  ( 9.000000000000017764, -12.50000000000000000, 5.000000000000007994 ) ) ;
#8660 =( NAMED_UNIT ( * ) PLANE_ANGLE_UNIT ( ) SI_UNIT ( $, .RADIAN. ) );
#8661 = DIRECTION ( 'NONE',  ( -1.848892746611746419E-31, -1.000000000000000000, 3.250006781153460502E-32 ) ) ;
#8662 = CARTESIAN_POINT ( 'NONE',  ( 2.000000000000001776, -1.773042676681341856, 3.469446951953614189E-15 ) ) ;
#8663 = EDGE_LOOP ( 'NONE', ( #7532, #10190, #12216 ) ) ;
#8664 = CARTESIAN_POINT ( 'NONE',  ( 19.99999999999999645, 0.000000000000000000, 0.000000000000000000 ) ) ;
#8665 = CARTESIAN_POINT ( 'NONE',  ( 20.00000000000000355, 8.524476791110679130, -16.77732469694377926 ) ) ;
#8666 = VERTEX_POINT ( 'NONE', #9217 ) ;
#8667 = EDGE_LOOP ( 'NONE', ( #1731, #980, #2058, #1837 ) ) ;
#8668 = FACE_OUTER_BOUND ( 'NONE', #6891, .T. ) ;
#8669 = VERTEX_POINT ( 'NONE', #3267 ) ;
#8670 = ORIENTED_EDGE ( 'NONE', *, *, #3692, .T. ) ;
#8671 = EDGE_CURVE ( 'NONE', #10853, #7453, #2418, .T. ) ;
#8672 = DIRECTION ( 'NONE',  ( -1.000000000000000000, 1.010728034814421376E-30, 1.090846720500930387E-30 ) ) ;
#8673 = VERTEX_POINT ( 'NONE', #4272 ) ;
#8674 = VECTOR ( 'NONE', #842, 1000.000000000000000 ) ;
#8675 = DIRECTION ( 'NONE',  ( -1.000000000000000000, 1.010728034814421376E-30, 1.090846720500930387E-30 ) ) ;
#8676 = DIRECTION ( 'NONE',  ( 0.000000000000000000, 0.000000000000000000, 1.000000000000000000 ) ) ;
#8677 = AXIS2_PLACEMENT_3D ( 'NONE', #1614, #5735, #11481 ) ;
#8678 = ORIENTED_EDGE ( 'NONE', *, *, #5447, .T. ) ;
#8679 = CARTESIAN_POINT ( 'NONE',  ( -45.00000000000013500, 30.00000000000000000, 2.000000000000007994 ) ) ;
#8680 = DIRECTION ( 'NONE',  ( 1.000000000000000000, -1.259148358202862343E-17, -5.075416248775500648E-17 ) ) ;
#8681 = ORIENTED_EDGE ( 'NONE', *, *, #8796, .T. ) ;
#8682 = VERTEX_POINT ( 'NONE', #2483 ) ;
#8683 = CIRCLE ( 'NONE', #2748, 7.400000000000009237 ) ;
#8684 = VERTEX_POINT ( 'NONE', #1304 ) ;
#8685 = FACE_OUTER_BOUND ( 'NONE', #11770, .T. ) ;
#8686 = VERTEX_POINT ( 'NONE', #8196 ) ;
#8687 = DIRECTION ( 'NONE',  ( -1.000000000000000000, 1.010728034814421376E-30, 1.090846720500930387E-30 ) ) ;
#8688 = FACE_BOUND ( 'NONE', #8932, .T. ) ;
#8689 = VECTOR ( 'NONE', #5493, 1000.000000000000000 ) ;
#8690 = EDGE_CURVE ( 'NONE', #364, #11848, #703, .T. ) ;
#8691 = CIRCLE ( 'NONE', #5408, 2.800000000000003819 ) ;
#8692 = EDGE_CURVE ( 'NONE', #5655, #8777, #5240, .T. ) ;
#8693 = ADVANCED_FACE ( 'NONE', ( #2223 ), #4411, .T. ) ;
#8694 = EDGE_CURVE ( 'NONE', #245, #10621, #7491, .T. ) ;
#8695 = FACE_OUTER_BOUND ( 'NONE', #11687, .T. ) ;
#8696 = LINE ( 'NONE', #6957, #9028 ) ;
#8697 = ORIENTED_EDGE ( 'NONE', *, *, #8644, .F. ) ;
#8698 = DIRECTION ( 'NONE',  ( -0.5000000000000061062, 1.060575238724902601E-16, -0.8660254037844351549 ) ) ;
#8699 = CIRCLE ( 'NONE', #8070, 2.800000000000002487 ) ;
#8700 = EDGE_CURVE ( 'NONE', #3532, #1182, #5429, .T. ) ;
#8701 = VERTEX_POINT ( 'NONE', #11168 ) ;
#8702 = AXIS2_PLACEMENT_3D ( 'NONE', #11286, #3568, #11553 ) ;
#8703 = FACE_OUTER_BOUND ( 'NONE', #7204, .T. ) ;
#8704 = VECTOR ( 'NONE', #12231, 1000.000000000000000 ) ;
#8705 = FILL_AREA_STYLE ('',( #8763 ) ) ;
#8706 = CARTESIAN_POINT ( 'NONE',  ( 19.99999999999999645, 0.000000000000000000, 0.000000000000000000 ) ) ;
#8707 = CARTESIAN_POINT ( 'NONE',  ( 19.99999999999997868, 1.531833341630222112, -6.396997380212695816 ) ) ;
#8708 = DIRECTION ( 'NONE',  ( -1.000000000000000000, 1.010728034814421376E-30, 1.090846720500930387E-30 ) ) ;
#8709 = AXIS2_PLACEMENT_3D ( 'NONE', #1888, #6671, #5881 ) ;
#8710 = DIRECTION ( 'NONE',  ( 0.000000000000000000, 0.000000000000000000, 1.000000000000000000 ) ) ;
#8711 = EDGE_CURVE ( 'NONE', #5309, #10795, #2353, .T. ) ;
#8712 = CARTESIAN_POINT ( 'NONE',  ( -2.927912186991283461E-13, -4.796980096169334296, -3.721999068284310930 ) ) ;
#8713 = DIRECTION ( 'NONE',  ( 0.000000000000000000, 0.1525077710325581370, 0.9883022714608525883 ) ) ;
#8714 = FACE_OUTER_BOUND ( 'NONE', #12510, .T. ) ;
#8715 = DIRECTION ( 'NONE',  ( -1.000000000000000000, 1.010728034814421376E-30, 1.090846720500930387E-30 ) ) ;
#8716 = EDGE_CURVE ( 'NONE', #9151, #3286, #5031, .T. ) ;
#8717 = DIRECTION ( 'NONE',  ( 1.000000000000000000, -0.000000000000000000, -0.000000000000000000 ) ) ;
#8718 = ORIENTED_EDGE ( 'NONE', *, *, #2404, .F. ) ;
#8719 = ORIENTED_EDGE ( 'NONE', *, *, #8561, .T. ) ;
#8720 = CARTESIAN_POINT ( 'NONE',  ( -11.83215956619923226, -30.00000000000000000, 1.999999999999999556 ) ) ;
#8721 = CARTESIAN_POINT ( 'NONE',  ( 19.99999999999997868, 6.613766744932294550, -3.319350756341939324 ) ) ;
#8722 = CARTESIAN_POINT ( 'NONE',  ( 14.00000000000000000, 30.00000000000000000, 0.000000000000000000 ) ) ;
#8723 = EDGE_CURVE ( 'NONE', #7062, #6148, #904, .T. ) ;
#8724 = FACE_OUTER_BOUND ( 'NONE', #4991, .T. ) ;
#8725 = ORIENTED_EDGE ( 'NONE', *, *, #2439, .T. ) ;
#8726 = AXIS2_PLACEMENT_3D ( 'NONE', #3205, #7115, #11036 ) ;
#8727 = PRODUCT_DEFINITION_SHAPE ( 'NONE', 'NONE',  #12756 ) ;
#8728 = ORIENTED_EDGE ( 'NONE', *, *, #12698, .F. ) ;
#8729 = VERTEX_POINT ( 'NONE', #1499 ) ;
#8730 = DIRECTION ( 'NONE',  ( -1.000000000000000000, -2.206481006425900381E-16, 8.674603474570138454E-17 ) ) ;
#8731 = ORIENTED_EDGE ( 'NONE', *, *, #1114, .F. ) ;
#8732 = VECTOR ( 'NONE', #10496, 1000.000000000000000 ) ;
#8733 = ORIENTED_EDGE ( 'NONE', *, *, #8251, .T. ) ;
#8734 = AXIS2_PLACEMENT_3D ( 'NONE', #11704, #11839, #1911 ) ;
#8735 =( LENGTH_UNIT ( ) NAMED_UNIT ( * ) SI_UNIT ( .MILLI., .METRE. ) );
#8736 = CARTESIAN_POINT ( 'NONE',  ( 0.000000000000000000, -6.133480037816505082, 2.376659734729468010 ) ) ;
#8737 = EDGE_LOOP ( 'NONE', ( #1949, #11386, #6651, #4429, #1406, #9772 ) ) ;
#8738 = CARTESIAN_POINT ( 'NONE',  ( 0.000000000000000000, 6.544726022087258066, 0.6592800351837291295 ) ) ;
#8739 = CYLINDRICAL_SURFACE ( 'NONE', #9735, 2.500000000000003553 ) ;
#8740 = VERTEX_POINT ( 'NONE', #9344 ) ;
#8741 = FACE_OUTER_BOUND ( 'NONE', #4810, .T. ) ;
#8742 = CARTESIAN_POINT ( 'NONE',  ( 19.99999999999999645, -3.178467454237171363, 5.758943784352557493 ) ) ;
#8743 = VECTOR ( 'NONE', #6927, 1000.000000000000000 ) ;
#8744 = ORIENTED_EDGE ( 'NONE', *, *, #5335, .T. ) ;
#8745 = EDGE_CURVE ( 'NONE', #11042, #7319, #5842, .T. ) ;
#8746 = ORIENTED_EDGE ( 'NONE', *, *, #12415, .F. ) ;
#8747 = ORIENTED_EDGE ( 'NONE', *, *, #1607, .T. ) ;
#8748 = DIRECTION ( 'NONE',  ( 0.000000000000000000, 0.000000000000000000, -1.000000000000000000 ) ) ;
#8749 = CIRCLE ( 'NONE', #3223, 3.000000000000005773 ) ;
#8750 = ORIENTED_EDGE ( 'NONE', *, *, #11401, .F. ) ;
#8751 = AXIS2_PLACEMENT_3D ( 'NONE', #782, #8648, #6533 ) ;
#8752 = DIRECTION ( 'NONE',  ( -1.000000000000000000, 1.006188713385347367E-17, 3.844790828812615713E-17 ) ) ;
#8753 = ORIENTED_EDGE ( 'NONE', *, *, #4877, .F. ) ;
#8754 = DIRECTION ( 'NONE',  ( 0.000000000000000000, -1.000000000000000000, 8.560894001270036306E-16 ) ) ;
#8755 = DIRECTION ( 'NONE',  ( -4.683861624749751464E-31, -0.4338837391175658365, 0.9009688679024154823 ) ) ;
#8756 = CARTESIAN_POINT ( 'NONE',  ( 19.99999999999997868, 6.321830586517952710, -1.817291089601262621 ) ) ;
#8757 = ORIENTED_EDGE ( 'NONE', *, *, #9398, .T. ) ;
#8758 = CARTESIAN_POINT ( 'NONE',  ( 4.154306624730862652, 2.398490048084779502, -3.721999068284283396 ) ) ;
#8759 = ORIENTED_EDGE ( 'NONE', *, *, #12744, .T. ) ;
#8760 = CARTESIAN_POINT ( 'NONE',  ( 19.99999999999999645, 0.000000000000000000, 0.000000000000000000 ) ) ;
#8761 = EDGE_CURVE ( 'NONE', #1828, #5156, #3636, .T. ) ;
#8762 = EDGE_CURVE ( 'NONE', #7580, #9207, #784, .T. ) ;
#8763 = FILL_AREA_STYLE_COLOUR ( '', #12379 ) ;
#8764 = CARTESIAN_POINT ( 'NONE',  ( 0.000000000000000000, 0.2110513566294476284, -7.396989747516558467 ) ) ;
#8765 = VECTOR ( 'NONE', #4799, 1000.000000000000000 ) ;
#8766 = DIRECTION ( 'NONE',  ( -1.000000000000000000, 1.010728034814421376E-30, 1.090846720500930387E-30 ) ) ;
#8767 = MECHANICAL_DESIGN_GEOMETRIC_PRESENTATION_REPRESENTATION (  '', ( #2611 ), #9161 ) ;
#8768 = DIRECTION ( 'NONE',  ( 0.000000000000000000, 0.3513748240813434620, -0.9362348706397368714 ) ) ;
#8769 = DIRECTION ( 'NONE',  ( -0.000000000000000000, -1.000000000000000000, -0.000000000000000000 ) ) ;
#8770 = CARTESIAN_POINT ( 'NONE',  ( 14.00000000000000000, -30.00000000000000000, 0.000000000000000000 ) ) ;
#8771 = CYLINDRICAL_SURFACE ( 'NONE', #8625, 2.149999999999999023 ) ;
#8772 = DIRECTION ( 'NONE',  ( -1.000000000000000000, -1.031065855027150586E-29, 2.218671295934095703E-30 ) ) ;
#8773 = AXIS2_PLACEMENT_3D ( 'NONE', #4207, #6200, #9155 ) ;
#8774 = AXIS2_PLACEMENT_3D ( 'NONE', #1889, #10642, #5817 ) ;
#8775 = CARTESIAN_POINT ( 'NONE',  ( -31.74999999999995026, 1.110223024625157033E-16, 2.000000000000010214 ) ) ;
#8776 = PRODUCT_RELATED_PRODUCT_CATEGORY ( 'part', '', ( #6601 ) ) ;
#8777 = VERTEX_POINT ( 'NONE', #12333 ) ;
#8778 = ORIENTED_EDGE ( 'NONE', *, *, #3549, .F. ) ;
#8779 = DIRECTION ( 'NONE',  ( 0.000000000000000000, 0.000000000000000000, -1.000000000000000000 ) ) ;
#8780 = CARTESIAN_POINT ( 'NONE',  ( 32.99999999999999289, 40.41548023366552655, -10.14535464186970692 ) ) ;
#8781 = CYLINDRICAL_SURFACE ( 'NONE', #5732, 4.000000000000000000 ) ;
#8782 = VECTOR ( 'NONE', #5224, 1000.000000000000000 ) ;
#8783 = DIRECTION ( 'NONE',  ( 1.000000000000000000, 1.849040895279789448E-31, -6.938893903907224680E-17 ) ) ;
#8784 = ORIENTED_EDGE ( 'NONE', *, *, #10392, .F. ) ;
#8785 = AXIS2_PLACEMENT_3D ( 'NONE', #654, #9397, #5495 ) ;
#8786 = CARTESIAN_POINT ( 'NONE',  ( -2.499999999999999556, 3.061616997868382648E-16, 3.469446951953614189E-15 ) ) ;
#8787 = PLANE ( 'NONE',  #11011 ) ;
#8788 = ORIENTED_EDGE ( 'NONE', *, *, #9954, .F. ) ;
#8789 = ORIENTED_EDGE ( 'NONE', *, *, #5150, .F. ) ;
#8790 = DIRECTION ( 'NONE',  ( -1.000000000000000000, 1.010728034814421376E-30, 1.090846720500930387E-30 ) ) ;
#8791 = EDGE_LOOP ( 'NONE', ( #9764, #5473, #1906, #1898 ) ) ;
#8792 = EDGE_LOOP ( 'NONE', ( #7635, #12537, #2719, #11955 ) ) ;
#8793 = PRODUCT_CONTEXT ( 'NONE', #6838, 'mechanical' ) ;
#8794 = EDGE_CURVE ( 'NONE', #10905, #9298, #3354, .T. ) ;
#8795 = VECTOR ( 'NONE', #5715, 1000.000000000000000 ) ;
#8796 = EDGE_CURVE ( 'NONE', #12099, #6234, #7492, .T. ) ;
#8797 = FACE_OUTER_BOUND ( 'NONE', #1130, .T. ) ;
#8798 = VERTEX_POINT ( 'NONE', #10509 ) ;
#8799 = DIRECTION ( 'NONE',  ( -1.140150527077241873E-30, 0.000000000000000000, 1.000000000000000000 ) ) ;
#8800 = CARTESIAN_POINT ( 'NONE',  ( 27.00000000000001066, 39.92642927056392210, -24.05727230799563898 ) ) ;
#8801 = ORIENTED_EDGE ( 'NONE', *, *, #7128, .T. ) ;
#8802 = CYLINDRICAL_SURFACE ( 'NONE', #5708, 7.400000000000010125 ) ;
#8803 = EDGE_CURVE ( 'NONE', #8365, #4835, #6256, .T. ) ;
#8804 = DIRECTION ( 'NONE',  ( 0.000000000000000000, 1.000000000000000000, 0.000000000000000000 ) ) ;
#8805 = ORIENTED_EDGE ( 'NONE', *, *, #3577, .F. ) ;
#8806 = ORIENTED_EDGE ( 'NONE', *, *, #2792, .T. ) ;
#8807 = ORIENTED_EDGE ( 'NONE', *, *, #11639, .T. ) ;
#8808 = CARTESIAN_POINT ( 'NONE',  ( 0.000000000000000000, 6.544726022087268724, -0.6592800351836389794 ) ) ;
#8809 = ORIENTED_EDGE ( 'NONE', *, *, #9331, .T. ) ;
#8810 = FACE_OUTER_BOUND ( 'NONE', #9495, .T. ) ;
#8811 = AXIS2_PLACEMENT_3D ( 'NONE', #8607, #4687, #5587 ) ;
#8812 = EDGE_LOOP ( 'NONE', ( #2048, #10914, #11972, #10775 ) ) ;
#8813 = CARTESIAN_POINT ( 'NONE',  ( 4.200000000000001954, 0.000000000000000000, 1.999999999999983569 ) ) ;
#8814 = VECTOR ( 'NONE', #11987, 1000.000000000000000 ) ;
#8815 = DIRECTION ( 'NONE',  ( -0.8660254037844377084, -0.5000000000000015543, 1.972152263052529295E-31 ) ) ;
#8816 = ORIENTED_EDGE ( 'NONE', *, *, #3741, .T. ) ;
#8817 = VECTOR ( 'NONE', #12489, 1000.000000000000000 ) ;
#8818 = PLANE ( 'NONE',  #2909 ) ;
#8819 = ORIENTED_EDGE ( 'NONE', *, *, #6575, .F. ) ;
#8820 = DIRECTION ( 'NONE',  ( 1.000000000000000000, 1.031065855027150586E-29, 2.218671295934092550E-30 ) ) ;
#8821 = DIRECTION ( 'NONE',  ( -0.000000000000000000, -1.000000000000000000, -0.000000000000000000 ) ) ;
#8822 = VECTOR ( 'NONE', #7747, 1000.000000000000000 ) ;
#8823 = AXIS2_PLACEMENT_3D ( 'NONE', #7521, #4566, #8478 ) ;
#8824 = FACE_OUTER_BOUND ( 'NONE', #4576, .T. ) ;
#8825 = DIRECTION ( 'NONE',  ( -6.938893903907235773E-17, 0.000000000000000000, -1.000000000000000000 ) ) ;
#8826 = DIRECTION ( 'NONE',  ( 0.000000000000000000, 0.9883022714608525883, -0.1525077710325583313 ) ) ;
#8827 = EDGE_CURVE ( 'NONE', #3706, #11297, #8099, .T. ) ;
#8828 = CARTESIAN_POINT ( 'NONE',  ( -3.999999999999990674, -0.7890432684750864345, -0.04868663549881568908 ) ) ;
#8829 = DIRECTION ( 'NONE',  ( -1.000000000000000000, 1.010728034814421376E-30, 1.090846720500930387E-30 ) ) ;
#8830 = DIRECTION ( 'NONE',  ( 0.000000000000000000, 0.000000000000000000, -1.000000000000000000 ) ) ;
#8831 = CIRCLE ( 'NONE', #3708, 2.800000000000003819 ) ;
#8832 = AXIS2_PLACEMENT_3D ( 'NONE', #2075, #1101, #9973 ) ;
#8833 = AXIS2_PLACEMENT_3D ( 'NONE', #2231, #7887, #10063 ) ;
#8834 = DIRECTION ( 'NONE',  ( -0.000000000000000000, -1.000000000000000000, -0.000000000000000000 ) ) ;
#8835 = ORIENTED_EDGE ( 'NONE', *, *, #8692, .F. ) ;
#8836 = CARTESIAN_POINT ( 'NONE',  ( 0.000000000000000000, 4.596015818000077857, 4.705818469689517336 ) ) ;
#8837 = DIRECTION ( 'NONE',  ( -0.000000000000000000, -0.000000000000000000, 1.000000000000000000 ) ) ;
#8838 = CIRCLE ( 'NONE', #4946, 2.800000000000003819 ) ;
#8839 = DIRECTION ( 'NONE',  ( 0.9396926207859138680, 1.150791560227856926E-16, -0.3420201433256536139 ) ) ;
#8840 = VECTOR ( 'NONE', #11763, 1000.000000000000000 ) ;
#8841 = CARTESIAN_POINT ( 'NONE',  ( 19.99999999999999645, -2.401522331692910850, 6.999477872697376313 ) ) ;
#8842 = ORIENTED_EDGE ( 'NONE', *, *, #8803, .T. ) ;
#8843 = ADVANCED_FACE ( 'NONE', ( #2679 ), #8452, .T. ) ;
#8844 = FACE_OUTER_BOUND ( 'NONE', #11523, .T. ) ;
#8845 = EDGE_CURVE ( 'NONE', #5492, #8301, #1758, .T. ) ;
#8846 = EDGE_CURVE ( 'NONE', #12605, #3108, #7296, .T. ) ;
#8847 = DIRECTION ( 'NONE',  ( 0.000000000000000000, -1.000000000000000000, 1.467581828789149532E-15 ) ) ;
#8848 = LINE ( 'NONE', #6867, #11334 ) ;
#8849 = ORIENTED_EDGE ( 'NONE', *, *, #4952, .F. ) ;
#8850 = EDGE_LOOP ( 'NONE', ( #5191, #5248, #2778, #6887 ) ) ;
#8851 = CARTESIAN_POINT ( 'NONE',  ( 8.000000000000000000, 30.00000000000000000, -7.347880794884119736E-16 ) ) ;
#8852 = ORIENTED_EDGE ( 'NONE', *, *, #578, .F. ) ;
#8853 =( GEOMETRIC_REPRESENTATION_CONTEXT ( 3 ) GLOBAL_UNCERTAINTY_ASSIGNED_CONTEXT ( ( #2517 ) ) GLOBAL_UNIT_ASSIGNED_CONTEXT ( ( #10299, #1358, #12132 ) ) REPRESENTATION_CONTEXT ( 'NONE', 'WORKASPACE' ) );
#8854 = VERTEX_POINT ( 'NONE', #7684 ) ;
#8855 = EDGE_CURVE ( 'NONE', #6259, #9874, #8513, .T. ) ;
#8856 = DIRECTION ( 'NONE',  ( 0.000000000000000000, -0.6579387259397027066, -0.7530714660036197383 ) ) ;
#8857 = ORIENTED_EDGE ( 'NONE', *, *, #4127, .F. ) ;
#8858 = SURFACE_SIDE_STYLE ('',( #10915 ) ) ;
#8859 = CARTESIAN_POINT ( 'NONE',  ( 19.99999999999999645, 0.3649881613860001539, 6.567714405409708078 ) ) ;
#8860 = ORIENTED_EDGE ( 'NONE', *, *, #6011, .F. ) ;
#8861 = CARTESIAN_POINT ( 'NONE',  ( 0.000000000000000000, -4.621065432155046615, -4.569765340993108715 ) ) ;
#8862 = DIRECTION ( 'NONE',  ( -1.000000000000000000, 1.010728034814421376E-30, 1.090846720500930387E-30 ) ) ;
#8863 =( GEOMETRIC_REPRESENTATION_CONTEXT ( 3 ) GLOBAL_UNCERTAINTY_ASSIGNED_CONTEXT ( ( #5594 ) ) GLOBAL_UNIT_ASSIGNED_CONTEXT ( ( #2132, #4968, #5161 ) ) REPRESENTATION_CONTEXT ( 'NONE', 'WORKASPACE' ) );
#8864 = VERTEX_POINT ( 'NONE', #4659 ) ;
#8865 = EDGE_LOOP ( 'NONE', ( #11634, #5518, #2438, #10296, #10843, #829, #8090, #3839 ) ) ;
#8866 = ORIENTED_EDGE ( 'NONE', *, *, #9651, .F. ) ;
#8867 = CARTESIAN_POINT ( 'NONE',  ( 27.00000000000000355, 32.50906206197875292, -8.925292473609250266 ) ) ;
#8868 = EDGE_CURVE ( 'NONE', #8334, #3019, #6467, .T. ) ;
#8869 = AXIS2_PLACEMENT_3D ( 'NONE', #727, #3702, #10449 ) ;
#8870 = ORIENTED_EDGE ( 'NONE', *, *, #8296, .T. ) ;
#8871 = CARTESIAN_POINT ( 'NONE',  ( 33.00000000000001421, 81.84122341717352356, -27.68198508464163510 ) ) ;
#8872 = ORIENTED_EDGE ( 'NONE', *, *, #11724, .F. ) ;
#8873 = CONICAL_SURFACE ( 'NONE', #9273, 4.000000000000000000, 0.8911886515913786111 ) ;
#8874 = EDGE_CURVE ( 'NONE', #12600, #444, #9593, .T. ) ;
#8875 = EDGE_CURVE ( 'NONE', #1901, #5655, #5228, .T. ) ;
#8876 = CARTESIAN_POINT ( 'NONE',  ( 33.00000000000001421, 81.84122341717352356, -42.68198508464162444 ) ) ;
#8877 = CIRCLE ( 'NONE', #2940, 2.800000000000004263 ) ;
#8878 = PLANE ( 'NONE',  #2469 ) ;
#8879 = ORIENTED_EDGE ( 'NONE', *, *, #12719, .F. ) ;
#8880 = CARTESIAN_POINT ( 'NONE',  ( 2.000000000000001776, -0.8865213383406691516, 1.535500000000002085 ) ) ;
#8881 = ORIENTED_EDGE ( 'NONE', *, *, #7620, .F. ) ;
#8882 = CARTESIAN_POINT ( 'NONE',  ( -31.74999999999995026, 4.286263797015736595E-16, -3.500000000000017319 ) ) ;
#8883 = DIRECTION ( 'NONE',  ( 0.000000000000000000, 0.000000000000000000, 1.000000000000000000 ) ) ;
#8884 = AXIS2_PLACEMENT_3D ( 'NONE', #8760, #11799, #2986 ) ;
#8885 = LINE ( 'NONE', #2990, #11148 ) ;
#8886 = DIRECTION ( 'NONE',  ( -1.000000000000000000, 1.010728034814421376E-30, 1.090846720500930387E-30 ) ) ;
#8887 = CYLINDRICAL_SURFACE ( 'NONE', #4261, 6.999999999999999112 ) ;
#8888 = DIRECTION ( 'NONE',  ( 0.000000000000000000, 1.530455820933490821E-32, -1.000000000000000000 ) ) ;
#8889 = DIRECTION ( 'NONE',  ( 1.405158487424925176E-30, -0.3513748240813304724, -0.9362348706397417564 ) ) ;
#8890 = AXIS2_PLACEMENT_3D ( 'NONE', #3505, #5424, #12262 ) ;
#8891 = EDGE_CURVE ( 'NONE', #10207, #1374, #6723, .T. ) ;
#8892 = VECTOR ( 'NONE', #1918, 1000.000000000000000 ) ;
#8893 = CARTESIAN_POINT ( 'NONE',  ( -18.00000000000001421, -30.00000000000001421, 3.000000000000008438 ) ) ;
#8894 = CARTESIAN_POINT ( 'NONE',  ( 19.99999999999997868, -7.399010254356654492, 0.1210258481698887889 ) ) ;
#8895 = EDGE_CURVE ( 'NONE', #4665, #1508, #4601, .T. ) ;
#8896 = VECTOR ( 'NONE', #1190, 1000.000000000000000 ) ;
#8897 = ORIENTED_EDGE ( 'NONE', *, *, #7941, .F. ) ;
#8898 = CYLINDRICAL_SURFACE ( 'NONE', #1699, 2.800000000000003819 ) ;
#8899 = DIRECTION ( 'NONE',  ( -1.000000000000000000, 1.010728034814421376E-30, 1.090846720500930387E-30 ) ) ;
#8900 = CARTESIAN_POINT ( 'NONE',  ( 0.000000000000000000, -4.907279493584705499, -4.380262188593400552 ) ) ;
#8901 = DIRECTION ( 'NONE',  ( -1.244921116051907329E-30, 0.2660368455666687892, 0.9639628606958550172 ) ) ;
#8902 = DIRECTION ( 'NONE',  ( -1.000000000000000000, 1.010728034814421376E-30, 1.090846720500930387E-30 ) ) ;
#8903 = ORIENTED_EDGE ( 'NONE', *, *, #12265, .T. ) ;
#8904 = CARTESIAN_POINT ( 'NONE',  ( 0.000000000000000000, 6.018220532833765901, 2.453165835849275389 ) ) ;
#8905 = EDGE_CURVE ( 'NONE', #9566, #4626, #3399, .T. ) ;
#8906 = CARTESIAN_POINT ( 'NONE',  ( 0.000000000000000000, 0.000000000000000000, 0.000000000000000000 ) ) ;
#8907 = CYLINDRICAL_SURFACE ( 'NONE', #4883, 6.999999999999999112 ) ;
#8908 = VERTEX_POINT ( 'NONE', #5745 ) ;
#8909 = VECTOR ( 'NONE', #1363, 1000.000000000000000 ) ;
#8910 = ORIENTED_EDGE ( 'NONE', *, *, #5888, .T. ) ;
#8911 = CARTESIAN_POINT ( 'NONE',  ( 19.99999999999999645, -4.999339924971525129, -4.274890546384038537 ) ) ;
#8912 = ORIENTED_EDGE ( 'NONE', *, *, #9386, .F. ) ;
#8913 = VERTEX_POINT ( 'NONE', #538 ) ;
#8914 = PRODUCT_CONTEXT ( 'NONE', #2825, 'mechanical' ) ;
#8915 = EDGE_CURVE ( 'NONE', #12228, #11905, #4470, .T. ) ;
#8916 = DIRECTION ( 'NONE',  ( -1.000000000000000000, 1.010728034814421376E-30, 1.090846720500930387E-30 ) ) ;
#8917 = EDGE_CURVE ( 'NONE', #5257, #175, #2547, .T. ) ;
#8918 = ORIENTED_EDGE ( 'NONE', *, *, #8108, .F. ) ;
#8919 =( LENGTH_UNIT ( ) NAMED_UNIT ( * ) SI_UNIT ( .MILLI., .METRE. ) );
#8920 = EDGE_CURVE ( 'NONE', #8146, #11433, #1423, .T. ) ;
#8921 = DIRECTION ( 'NONE',  ( 0.000000000000000000, 1.000000000000000000, 0.000000000000000000 ) ) ;
#8922 = VERTEX_POINT ( 'NONE', #9908 ) ;
#8923 = CIRCLE ( 'NONE', #898, 4.000000000000000000 ) ;
#8924 = FACE_OUTER_BOUND ( 'NONE', #6087, .T. ) ;
#8925 = CARTESIAN_POINT ( 'NONE',  ( 19.99999999999999645, -4.357840574720558635, -4.821434073522041786 ) ) ;
#8926 = AXIS2_PLACEMENT_3D ( 'NONE', #5564, #594, #11429 ) ;
#8927 = ORIENTED_EDGE ( 'NONE', *, *, #213, .F. ) ;
#8928 = ORIENTED_EDGE ( 'NONE', *, *, #11767, .F. ) ;
#8929 = ORIENTED_EDGE ( 'NONE', *, *, #5794, .F. ) ;
#8930 = DIRECTION ( 'NONE',  ( 1.140150527077241873E-30, 0.000000000000000000, -1.000000000000000000 ) ) ;
#8931 = CARTESIAN_POINT ( 'NONE',  ( 11.00000000000003375, 12.50000000000000000, -4.062508476441825628E-31 ) ) ;
#8932 = EDGE_LOOP ( 'NONE', ( #12478, #8927 ) ) ;
#8933 = CYLINDRICAL_SURFACE ( 'NONE', #6777, 6.499000000000010324 ) ;
#8934 = ORIENTED_EDGE ( 'NONE', *, *, #8561, .F. ) ;
#8935 = AXIS2_PLACEMENT_3D ( 'NONE', #2793, #3803, #6707 ) ;
#8936 = AXIS2_PLACEMENT_3D ( 'NONE', #4816, #11461, #2642 ) ;
#8937 = DIRECTION ( 'NONE',  ( -1.140150527077241873E-30, 0.000000000000000000, 1.000000000000000000 ) ) ;
#8938 = EDGE_CURVE ( 'NONE', #3010, #477, #10879, .T. ) ;
#8939 = DIRECTION ( 'NONE',  ( -1.000000000000000000, 1.006188713385347367E-17, 3.844790828812615713E-17 ) ) ;
#8940 = CARTESIAN_POINT ( 'NONE',  ( 34.00000000000000000, 0.000000000000000000, -1.734723475976807094E-14 ) ) ;
#8941 = ORIENTED_EDGE ( 'NONE', *, *, #6280, .F. ) ;
#8942 = DIRECTION ( 'NONE',  ( 0.000000000000000000, 1.530455820933490821E-32, -1.000000000000000000 ) ) ;
#8943 = AXIS2_PLACEMENT_3D ( 'NONE', #897, #6956, #10866 ) ;
#8944 = VERTEX_POINT ( 'NONE', #5931 ) ;
#8945 = CIRCLE ( 'NONE', #3421, 1.535500000000001863 ) ;
#8946 = DIRECTION ( 'NONE',  ( 1.000000000000000000, 0.000000000000000000, -6.375108774214761023E-14 ) ) ;
#8947 = EDGE_CURVE ( 'NONE', #6820, #6211, #4723, .T. ) ;
#8948 = FACE_OUTER_BOUND ( 'NONE', #12423, .T. ) ;
#8949 = EDGE_CURVE ( 'NONE', #5688, #9218, #12547, .T. ) ;
#8950 = CARTESIAN_POINT ( 'NONE',  ( -17.00000000000000000, 2.632990618166785569E-16, 17.85000000000008313 ) ) ;
#8951 = CARTESIAN_POINT ( 'NONE',  ( -0.6937372685066772737, 4.453844082567717244, -3.610536846335900218 ) ) ;
#8952 = DIRECTION ( 'NONE',  ( 1.577021341797099039E-16, 1.177425296209237084E-30, 1.000000000000000000 ) ) ;
#8953 = EDGE_CURVE ( 'NONE', #1577, #8666, #1941, .T. ) ;
#8954 = LINE ( 'NONE', #5166, #3607 ) ;
#8955 = DIRECTION ( 'NONE',  ( 0.000000000000000000, 0.1785568947986370392, -0.9839295885986295565 ) ) ;
#8956 = DIRECTION ( 'NONE',  ( -1.000000000000000000, 0.000000000000000000, 0.000000000000000000 ) ) ;
#8957 = FACE_OUTER_BOUND ( 'NONE', #8791, .T. ) ;
#8958 =( REPRESENTATION_RELATIONSHIP ('NONE','NONE', #10018, #10094 ) REPRESENTATION_RELATIONSHIP_WITH_TRANSFORMATION ( #6336 )SHAPE_REPRESENTATION_RELATIONSHIP( ) );
#8959 =( GEOMETRIC_REPRESENTATION_CONTEXT ( 3 ) GLOBAL_UNCERTAINTY_ASSIGNED_CONTEXT ( ( #2873 ) ) GLOBAL_UNIT_ASSIGNED_CONTEXT ( ( #11195, #8474, #8289 ) ) REPRESENTATION_CONTEXT ( 'NONE', 'WORKASPACE' ) );
#8960 = ORIENTED_EDGE ( 'NONE', *, *, #4861, .F. ) ;
#8961 = LINE ( 'NONE', #10046, #7463 ) ;
#8962 = DIRECTION ( 'NONE',  ( -1.000000000000000000, 1.010728034814421376E-30, 1.090846720500930387E-30 ) ) ;
#8963 = CARTESIAN_POINT ( 'NONE',  ( 19.99999999999999645, 0.000000000000000000, 0.000000000000000000 ) ) ;
#8964 = DIRECTION ( 'NONE',  ( 0.000000000000000000, 0.000000000000000000, -1.000000000000000000 ) ) ;
#8965 = CARTESIAN_POINT ( 'NONE',  ( 0.000000000000000000, 5.956456411769377901, 2.790827096699005416 ) ) ;
#8966 = ORIENTED_EDGE ( 'NONE', *, *, #11169, .T. ) ;
#8967 = LINE ( 'NONE', #4987, #10800 ) ;
#8968 = CIRCLE ( 'NONE', #7535, 3.500000000000003997 ) ;
#8969 = CARTESIAN_POINT ( 'NONE',  ( 0.000000000000000000, 0.8865213383406622683, -1.535499999999995202 ) ) ;
#8970 = AXIS2_PLACEMENT_3D ( 'NONE', #12159, #4284, #8213 ) ;
#8971 = CARTESIAN_POINT ( 'NONE',  ( -17.00000000000000000, 0.000000000000000000, 20.00000000000007461 ) ) ;
#8972 = ORIENTED_EDGE ( 'NONE', *, *, #2477, .F. ) ;
#8973 = EDGE_LOOP ( 'NONE', ( #8429, #6856, #6146, #6755 ) ) ;
#8974 = CARTESIAN_POINT ( 'NONE',  ( 0.000000000000000000, 4.618802153516985420, -3.433295621305398893 ) ) ;
#8975 = VERTEX_POINT ( 'NONE', #10696 ) ;
#8976 = ORIENTED_EDGE ( 'NONE', *, *, #9225, .T. ) ;
#8977 = APPLICATION_PROTOCOL_DEFINITION ( 'draft international standard', 'automotive_design', 1998, #1732 ) ;
#8978 = DIRECTION ( 'NONE',  ( -1.000000000000000000, 0.000000000000000000, 0.000000000000000000 ) ) ;
#8979 = EDGE_LOOP ( 'NONE', ( #11563, #10536, #9915, #11858 ) ) ;
#8980 = CIRCLE ( 'NONE', #2620, 7.400000000000011902 ) ;
#8981 = LINE ( 'NONE', #12680, #12339 ) ;
#8982 = CYLINDRICAL_SURFACE ( 'NONE', #11383, 2.800000000000003819 ) ;
#8983 = ORIENTED_EDGE ( 'NONE', *, *, #4062, .F. ) ;
#8984 = CARTESIAN_POINT ( 'NONE',  ( 19.99999999999999645, 5.012092988313947117, 4.137139697483554812 ) ) ;
#8985 = LINE ( 'NONE', #6218, #4893 ) ;
#8986 = CARTESIAN_POINT ( 'NONE',  ( 19.99999999999997868, -1.966014849756994254, -6.277170897746295886 ) ) ;
#8987 = EDGE_CURVE ( 'NONE', #6567, #9408, #2073, .T. ) ;
#8988 = B_SPLINE_CURVE_WITH_KNOTS ( 'NONE', 3,
 ( #6934, #4023, #5954, #1055, #7945, #6993 ),
 .UNSPECIFIED., .F., .F.,
 ( 4, 2, 4 ),
 ( -3.640115492411093008E-06, 0.0002066546034003419164, 0.0004169493222930948902 ),
 .UNSPECIFIED. ) ;
#8989 = ORIENTED_EDGE ( 'NONE', *, *, #6604, .F. ) ;
#8990 = ORIENTED_EDGE ( 'NONE', *, *, #5405, .T. ) ;
#8991 = AXIS2_PLACEMENT_3D ( 'NONE', #7261, #11181, #6028 ) ;
#8992 = EDGE_LOOP ( 'NONE', ( #7900, #4730 ) ) ;
#8993 = ORIENTED_EDGE ( 'NONE', *, *, #8503, .F. ) ;
#8994 = LINE ( 'NONE', #1074, #4998 ) ;
#8995 = CARTESIAN_POINT ( 'NONE',  ( 4.000000000000001776, 0.8228435280417438769, -3.430609588141305899 ) ) ;
#8996 = VERTEX_POINT ( 'NONE', #3120 ) ;
#8997 = CARTESIAN_POINT ( 'NONE',  ( 4.000000000000000000, 0.3987449864460003712, -0.01220643443059823453 ) ) ;
#8998 = ORIENTED_EDGE ( 'NONE', *, *, #12320, .F. ) ;
#8999 = CARTESIAN_POINT ( 'NONE',  ( 4.000000000000003553, 0.000000000000000000, 0.000000000000000000 ) ) ;
#9000 = DIRECTION ( 'NONE',  ( -1.000000000000000000, 1.010728034814421376E-30, 1.090846720500930387E-30 ) ) ;
#9001 = EDGE_CURVE ( 'NONE', #5654, #4676, #12130, .T. ) ;
#9002 = PRODUCT_DEFINITION ( 'UNKNOWN', '', #12504, #4439 ) ;
#9003 = CARTESIAN_POINT ( 'NONE',  ( 9.999999999999998224, 7.164568425986761468, 1.851744925564471123 ) ) ;
#9004 = VERTEX_POINT ( 'NONE', #1100 ) ;
#9005 = DIRECTION ( 'NONE',  ( -1.000000000000000000, -1.081682119347366197E-16, 6.938893903907228378E-17 ) ) ;
#9006 = ORIENTED_EDGE ( 'NONE', *, *, #2187, .F. ) ;
#9007 = CARTESIAN_POINT ( 'NONE',  ( 0.000000000000000000, 0.000000000000000000, 0.000000000000000000 ) ) ;
#9008 = CARTESIAN_POINT ( 'NONE',  ( 11.00000000000003020, 30.00000000000000000, -9.742497179615118866E-31 ) ) ;
#9009 = DIRECTION ( 'NONE',  ( 0.000000000000000000, 0.000000000000000000, 1.000000000000000000 ) ) ;
#9010 = CARTESIAN_POINT ( 'NONE',  ( 0.000000000000000000, -1.966014849757081073, 6.277170897746257694 ) ) ;
#9011 = CARTESIAN_POINT ( 'NONE',  ( -31.74999999999995026, 0.000000000000000000, -1.734723475976807094E-14 ) ) ;
#9012 = CIRCLE ( 'NONE', #9406, 4.000000000000000000 ) ;
#9013 = EDGE_CURVE ( 'NONE', #6234, #9770, #974, .T. ) ;
#9014 = DIRECTION ( 'NONE',  ( -1.000000000000000000, 1.010728034814421376E-30, 1.090846720500930387E-30 ) ) ;
#9015 = EDGE_CURVE ( 'NONE', #7169, #11765, #6577, .T. ) ;
#9016 = DIRECTION ( 'NONE',  ( 1.000000000000000000, -1.010728034814421376E-30, -1.090846720500930387E-30 ) ) ;
#9017 = B_SPLINE_CURVE_WITH_KNOTS ( 'NONE', 3,
 ( #449, #10095, #3246, #9262, #3371, #12186, #6122, #4380 ),
 .UNSPECIFIED., .F., .F.,
 ( 4, 2, 2, 4 ),
 ( 0.005725059856848637406, 0.006314084072593623143, 0.006903108288338608012, 0.008081156719828579485 ),
 .UNSPECIFIED. ) ;
#9018 = DIRECTION ( 'NONE',  ( -0.8191520442889875797, 1.003171929053519447E-16, 0.5735764363510522656 ) ) ;
#9019 = AXIS2_PLACEMENT_3D ( 'NONE', #5873, #2936, #3822 ) ;
#9020 = ADVANCED_FACE ( 'NONE', ( #9659 ), #8771, .F. ) ;
#9021 = ORIENTED_EDGE ( 'NONE', *, *, #9001, .F. ) ;
#9022 = FACE_OUTER_BOUND ( 'NONE', #10922, .T. ) ;
#9023 = CARTESIAN_POINT ( 'NONE',  ( 8.000000000000000000, 30.00000000000000000, -7.347880794884119736E-16 ) ) ;
#9024 = CYLINDRICAL_SURFACE ( 'NONE', #6135, 3.000000000000005773 ) ;
#9025 = DIRECTION ( 'NONE',  ( -2.126226658603505754E-31, 0.7818314824680310249, -0.6234898018587319291 ) ) ;
#9026 = ORIENTED_EDGE ( 'NONE', *, *, #1708, .T. ) ;
#9027 = CARTESIAN_POINT ( 'NONE',  ( 0.000000000000000000, 1.395418990828199757, 6.428133065596412621 ) ) ;
#9028 = VECTOR ( 'NONE', #1086, 1000.000000000000000 ) ;
#9029 =( GEOMETRIC_REPRESENTATION_CONTEXT ( 3 ) GLOBAL_UNCERTAINTY_ASSIGNED_CONTEXT ( ( #6603 ) ) GLOBAL_UNIT_ASSIGNED_CONTEXT ( ( #1565, #12078, #3330 ) ) REPRESENTATION_CONTEXT ( 'NONE', 'WORKASPACE' ) );
#9030 = AXIS2_PLACEMENT_3D ( 'NONE', #6147, #286, #9873 ) ;
#9031 = EDGE_CURVE ( 'NONE', #2105, #2119, #10821, .T. ) ;
#9032 = DIRECTION ( 'NONE',  ( -4.930380657631325535E-31, -1.000000000000000000, -1.177425296209239362E-30 ) ) ;
#9033 = EDGE_CURVE ( 'NONE', #6138, #9558, #1212, .T. ) ;
#9034 = CONICAL_SURFACE ( 'NONE', #12135, 1.610000000000000098, 0.7853981633974652654 ) ;
#9035 = EDGE_LOOP ( 'NONE', ( #4087, #6106, #9609, #868, #2565 ) ) ;
#9036 = CYLINDRICAL_SURFACE ( 'NONE', #10294, 7.400000000000010125 ) ;
#9037 = ORIENTED_EDGE ( 'NONE', *, *, #10367, .F. ) ;
#9038 = VERTEX_POINT ( 'NONE', #4006 ) ;
#9039 = SHAPE_DEFINITION_REPRESENTATION ( #7622, #71 ) ;
#9040 = COLOUR_RGB ( '', 0.09019608, 0.27058824, 0.51372549) ;
#9041 = DIRECTION ( 'NONE',  ( -0.000000000000000000, -1.000000000000000000, -0.000000000000000000 ) ) ;
#9042 = CIRCLE ( 'NONE', #10889, 6.499000000000009436 ) ;
#9043 = ORIENTED_EDGE ( 'NONE', *, *, #9158, .F. ) ;
#9044 = AXIS2_PLACEMENT_3D ( 'NONE', #10749, #5925, #4777 ) ;
#9045 = CARTESIAN_POINT ( 'NONE',  ( 6.000000000000000000, 49.63999999999998636, -13.00000000000000178 ) ) ;
#9046 = DIRECTION ( 'NONE',  ( 0.000000000000000000, 0.000000000000000000, 1.000000000000000000 ) ) ;
#9047 = ORIENTED_EDGE ( 'NONE', *, *, #7732, .T. ) ;
#9048 = DIRECTION ( 'NONE',  ( -1.000000000000000000, 1.006188713385347367E-17, 3.844790828812615713E-17 ) ) ;
#9049 = DIRECTION ( 'NONE',  ( 0.000000000000000000, -0.8345732537213080837, 0.5508969814520944253 ) ) ;
#9050 = DIRECTION ( 'NONE',  ( -1.140150527077241873E-30, 0.000000000000000000, 1.000000000000000000 ) ) ;
#9051 = CARTESIAN_POINT ( 'NONE',  ( 28.61000000000001009, 3.469446951953614189E-15, 0.000000000000000000 ) ) ;
#9052 = COLOUR_RGB ( '', 0.66274510, 0.83137255, 0.94901961) ;
#9053 = ORIENTED_EDGE ( 'NONE', *, *, #9491, .T. ) ;
#9054 = ORIENTED_EDGE ( 'NONE', *, *, #11251, .T. ) ;
#9055 = EDGE_CURVE ( 'NONE', #4761, #10601, #7394, .T. ) ;
#9056 = ORIENTED_EDGE ( 'NONE', *, *, #3740, .T. ) ;
#9057 = EDGE_LOOP ( 'NONE', ( #11975, #5276, #822, #5828 ) ) ;
#9058 = CARTESIAN_POINT ( 'NONE',  ( 19.99999999999999645, -6.133480037816472219, -2.376659734729558160 ) ) ;
#9059 = EDGE_CURVE ( 'NONE', #8468, #10149, #2886, .T. ) ;
#9060 = DIRECTION ( 'NONE',  ( 1.000000000000000000, 0.000000000000000000, 0.000000000000000000 ) ) ;
#9061 = ORIENTED_EDGE ( 'NONE', *, *, #9481, .T. ) ;
#9062 = CYLINDRICAL_SURFACE ( 'NONE', #10868, 7.400000000000010125 ) ;
#9063 = MECHANICAL_DESIGN_GEOMETRIC_PRESENTATION_REPRESENTATION (  '', ( #7841 ), #8863 ) ;
#9064 = VERTEX_POINT ( 'NONE', #7925 ) ;
#9065 = CARTESIAN_POINT ( 'NONE',  ( 19.99999999999999645, -2.099089055167807860, 6.233932467347772288 ) ) ;
#9066 = DIRECTION ( 'NONE',  ( -1.000000000000000000, 1.010728034814421376E-30, 1.090846720500930387E-30 ) ) ;
#9067 = CARTESIAN_POINT ( 'NONE',  ( 50.00005079999998969, 5.204170427930421283E-15, -6.938893903907228378E-15 ) ) ;
#9068 = ORIENTED_EDGE ( 'NONE', *, *, #2334, .T. ) ;
#9070 = CARTESIAN_POINT ( 'NONE',  ( 4.000000000000003553, 0.000000000000000000, 0.000000000000000000 ) ) ;
#9069 = CIRCLE ( 'NONE', #1678, 7.400000000000011902 ) ;
#9071 = VERTEX_POINT ( 'NONE', #78 ) ;
#9072 = CARTESIAN_POINT ( 'NONE',  ( 19.99999999999999645, 0.000000000000000000, 0.000000000000000000 ) ) ;
#9073 = EDGE_CURVE ( 'NONE', #12081, #8571, #1036, .T. ) ;
#9074 = CARTESIAN_POINT ( 'NONE',  ( -40.00000000000000000, 30.00000000000000000, 2.000000000000003109 ) ) ;
#9075 = EDGE_CURVE ( 'NONE', #4417, #7479, #3941, .T. ) ;
#9076 = EDGE_CURVE ( 'NONE', #7377, #6343, #9228, .T. ) ;
#9077 = AXIS2_PLACEMENT_3D ( 'NONE', #1934, #10946, #5033 ) ;
#9078 = CYLINDRICAL_SURFACE ( 'NONE', #3546, 1.000000000000001332 ) ;
#9079 = AXIS2_PLACEMENT_3D ( 'NONE', #9646, #649, #12580 ) ;
#9080 = CARTESIAN_POINT ( 'NONE',  ( 14.00000000000000000, 30.00000000000000000, 4.000000000000000000 ) ) ;
#9081 = DIRECTION ( 'NONE',  ( 0.000000000000000000, 0.000000000000000000, -1.000000000000000000 ) ) ;
#9082 = CARTESIAN_POINT ( 'NONE',  ( 2.500000000000035527, -3.469446951953657734E-14, -5.000000000000011546 ) ) ;
#9083 = DIRECTION ( 'NONE',  ( -3.437775699846481192E-17, -0.2951046417778634967, -0.9554649393887558739 ) ) ;
#9084 = CARTESIAN_POINT ( 'NONE',  ( 0.000000000000000000, -7.301715115245771770, -1.202063382601599395 ) ) ;
#9085 = CIRCLE ( 'NONE', #10945, 9.999999999999998224 ) ;
#9086 =( NAMED_UNIT ( * ) PLANE_ANGLE_UNIT ( ) SI_UNIT ( $, .RADIAN. ) );
#9087 = ADVANCED_FACE ( 'NONE', ( #8714, #2872 ), #2399, .T. ) ;
#9088 = ORIENTED_EDGE ( 'NONE', *, *, #4895, .F. ) ;
#9089 = PLANE ( 'NONE',  #6438 ) ;
#9090 = CARTESIAN_POINT ( 'NONE',  ( 19.99999999999999645, -5.651611091574776147, -4.776954267060665060 ) ) ;
#9091 = DIRECTION ( 'NONE',  ( -1.000000000000000000, 1.010728034814421376E-30, 1.090846720500930387E-30 ) ) ;
#9092 = DIRECTION ( 'NONE',  ( -1.000000000000000000, 1.010728034814421376E-30, 1.090846720500930387E-30 ) ) ;
#9093 = ORIENTED_EDGE ( 'NONE', *, *, #2169, .T. ) ;
#9094 = AXIS2_PLACEMENT_3D ( 'NONE', #2282, #1298, #6260 ) ;
#9095 = CYLINDRICAL_SURFACE ( 'NONE', #5463, 2.800000000000003819 ) ;
#9096 = AXIS2_PLACEMENT_3D ( 'NONE', #1330, #9245, #7139 ) ;
#9097 = CARTESIAN_POINT ( 'NONE',  ( 0.000000000000000000, -6.213893036447822205, 1.903820982021506403 ) ) ;
#9098 = EDGE_CURVE ( 'NONE', #7479, #1463, #10251, .T. ) ;
#9099 = VERTEX_POINT ( 'NONE', #4387 ) ;
#9100 = CARTESIAN_POINT ( 'NONE',  ( 40.00000000000000711, 18.52447679111068268, -16.77732469694377926 ) ) ;
#9101 = ORIENTED_EDGE ( 'NONE', *, *, #11543, .F. ) ;
#9102 = AXIS2_PLACEMENT_3D ( 'NONE', #10916, #5126, #9046 ) ;
#9103 = VERTEX_POINT ( 'NONE', #9082 ) ;
#9104 = ITEM_DEFINED_TRANSFORMATION ( 'NONE', 'NONE', #4467,  #12422 ) ;
#9105 = CIRCLE ( 'NONE', #8075, 7.400000000000009237 ) ;
#9106 = CARTESIAN_POINT ( 'NONE',  ( 19.99999999999997868, 2.520781513113738548, -6.075668640744172677 ) ) ;
#9107 = EDGE_LOOP ( 'NONE', ( #8993, #4707, #6772, #11384 ) ) ;
#9108 = EDGE_CURVE ( 'NONE', #753, #11058, #3438, .T. ) ;
#9109 = CARTESIAN_POINT ( 'NONE',  ( 10.00000000000000178, 6.613766744932252806, 3.319350756342029474 ) ) ;
#9110 = CARTESIAN_POINT ( 'NONE',  ( 0.000000000000000000, -6.289597356626462243, -3.898841506334620011 ) ) ;
#9111 = EDGE_CURVE ( 'NONE', #7500, #302, #5128, .T. ) ;
#9112 = EDGE_LOOP ( 'NONE', ( #1440, #11130, #10050, #5903 ) ) ;
#9113 = FACE_OUTER_BOUND ( 'NONE', #8865, .T. ) ;
#9114 = CARTESIAN_POINT ( 'NONE',  ( -3.999999999999991562, 2.309401076758501592, -4.999999999999993783 ) ) ;
#9115 = FACE_OUTER_BOUND ( 'NONE', #5844, .T. ) ;
#9116 = VECTOR ( 'NONE', #8837, 1000.000000000000000 ) ;
#9117 = ORIENTED_EDGE ( 'NONE', *, *, #10876, .T. ) ;
#9118 = ORIENTED_EDGE ( 'NONE', *, *, #7279, .F. ) ;
#9119 = ORIENTED_EDGE ( 'NONE', *, *, #1479, .T. ) ;
#9120 = VERTEX_POINT ( 'NONE', #3376 ) ;
#9121 = DIRECTION ( 'NONE',  ( -1.000000000000000000, 0.000000000000000000, 1.301042606982602363E-16 ) ) ;
#9122 = CIRCLE ( 'NONE', #8309, 7.400000000000011902 ) ;
#9123 = CARTESIAN_POINT ( 'NONE',  ( 4.000000000000001776, 2.512223110932509940, -3.469391141908801934 ) ) ;
#9124 = ORIENTED_EDGE ( 'NONE', *, *, #6057, .F. ) ;
#9125 = CARTESIAN_POINT ( 'NONE',  ( -40.00000000000000000, -19.99999999999999645, 2.831145448779744488E-15 ) ) ;
#9126 = VERTEX_POINT ( 'NONE', #8312 ) ;
#9127 = DIRECTION ( 'NONE',  ( -1.000000000000000000, 1.010728034814421376E-30, 1.090846720500930387E-30 ) ) ;
#9128 = VECTOR ( 'NONE', #5890, 1000.000000000000000 ) ;
#9129 = EDGE_CURVE ( 'NONE', #3793, #6015, #1010, .T. ) ;
#9130 = DIRECTION ( 'NONE',  ( -1.140150527077241873E-30, 0.000000000000000000, 1.000000000000000000 ) ) ;
#9131 = CARTESIAN_POINT ( 'NONE',  ( 2.000000000000001776, -0.8865213383406727043, 1.535500000000009191 ) ) ;
#9132 = ORIENTED_EDGE ( 'NONE', *, *, #12657, .T. ) ;
#9133 = FACE_OUTER_BOUND ( 'NONE', #3497, .T. ) ;
#9134 = ORIENTED_EDGE ( 'NONE', *, *, #7692, .T. ) ;
#9135 = DIRECTION ( 'NONE',  ( -1.000000000000000000, 1.010728034814421376E-30, 1.090846720500930387E-30 ) ) ;
#9136 = AXIS2_PLACEMENT_3D ( 'NONE', #6912, #5994, #5037 ) ;
#9137 = AXIS2_PLACEMENT_3D ( 'NONE', #8611, #5716, #6563 ) ;
#9138 = DIRECTION ( 'NONE',  ( 0.000000000000000000, -1.000000000000000000, 0.000000000000000000 ) ) ;
#9139 = DIRECTION ( 'NONE',  ( 0.000000000000000000, 1.530455820933490821E-32, -1.000000000000000000 ) ) ;
#9140 = PRODUCT_DEFINITION_SHAPE ( 'NONE', 'NONE',  #2659 ) ;
#9141 = DIRECTION ( 'NONE',  ( 0.000000000000000000, 0.08963930890342669544, 0.9959742939952396235 ) ) ;
#9142 = CARTESIAN_POINT ( 'NONE',  ( 9.000000000000031974, -6.123233995736753463E-16, 20.00000000000003553 ) ) ;
#9143 = CIRCLE ( 'NONE', #1751, 2.800000000000003819 ) ;
#9144 = AXIS2_PLACEMENT_3D ( 'NONE', #4882, #11900, #8804 ) ;
#9145 = DIRECTION ( 'NONE',  ( 1.000000000000000000, 1.849040895279789448E-31, -6.938893903907224680E-17 ) ) ;
#9146 = EDGE_CURVE ( 'NONE', #10923, #8777, #3093, .T. ) ;
#9147 = CARTESIAN_POINT ( 'NONE',  ( 33.00000000000001421, 39.49790820824818383, -24.06186359251418594 ) ) ;
#9148 = ADVANCED_FACE ( 'NONE', ( #4195 ), #12255, .T. ) ;
#9149 = LINE ( 'NONE', #2279, #4148 ) ;
#9150 =( NAMED_UNIT ( * ) SI_UNIT ( $, .STERADIAN. ) SOLID_ANGLE_UNIT ( ) );
#9151 = VERTEX_POINT ( 'NONE', #8116 ) ;
#9152 = CARTESIAN_POINT ( 'NONE',  ( 28.99999999999999645, 3.558819905435939259E-15, 1.610000000000001874 ) ) ;
#9153 = CARTESIAN_POINT ( 'NONE',  ( 19.99999999999999645, 0.000000000000000000, 0.000000000000000000 ) ) ;
#9154 = DIRECTION ( 'NONE',  ( 0.000000000000000000, 0.000000000000000000, 1.000000000000000000 ) ) ;
#9155 = DIRECTION ( 'NONE',  ( 0.000000000000000000, 0.000000000000000000, 1.000000000000000000 ) ) ;
#9156 = CARTESIAN_POINT ( 'NONE',  ( 0.000000000000000000, -3.399584271718293582, -6.572885726945646212 ) ) ;
#9157 = CARTESIAN_POINT ( 'NONE',  ( 12.94787914004602847, -12.49999999999999645, 5.638155724715463002 ) ) ;
#9158 = EDGE_CURVE ( 'NONE', #10545, #1458, #6355, .T. ) ;
#9159 = PRODUCT_RELATED_PRODUCT_CATEGORY ( 'part', '', ( #10271 ) ) ;
#9160 = ORIENTED_EDGE ( 'NONE', *, *, #12188, .F. ) ;
#9161 =( GEOMETRIC_REPRESENTATION_CONTEXT ( 3 ) GLOBAL_UNCERTAINTY_ASSIGNED_CONTEXT ( ( #5682 ) ) GLOBAL_UNIT_ASSIGNED_CONTEXT ( ( #5312, #6091, #5130 ) ) REPRESENTATION_CONTEXT ( 'NONE', 'WORKASPACE' ) );
#9162 = CARTESIAN_POINT ( 'NONE',  ( 9.999999999999994671, -6.884685972239644514, -2.713134545806128450 ) ) ;
#9163 = ORIENTED_EDGE ( 'NONE', *, *, #6435, .T. ) ;
#9164 = ORIENTED_EDGE ( 'NONE', *, *, #11877, .T. ) ;
#9165 = VERTEX_POINT ( 'NONE', #12062 ) ;
#9166 = DIRECTION ( 'NONE',  ( 0.000000000000000000, -0.2660368455666824450, 0.9639628606958512425 ) ) ;
#9167 = DIRECTION ( 'NONE',  ( 0.000000000000000000, 0.000000000000000000, 1.000000000000000000 ) ) ;
#9168 = FACE_OUTER_BOUND ( 'NONE', #2183, .T. ) ;
#9169 = VECTOR ( 'NONE', #11440, 1000.000000000000000 ) ;
#9170 = CARTESIAN_POINT ( 'NONE',  ( 19.99999999999999645, -3.426907987218856810, 5.522074125465504579 ) ) ;
#9171 = AXIS2_PLACEMENT_3D ( 'NONE', #8963, #1364, #338 ) ;
#9172 = FACE_OUTER_BOUND ( 'NONE', #11813, .T. ) ;
#9173 = ADVANCED_FACE ( 'NONE', ( #3252, #11086 ), #7355, .T. ) ;
#9174 = DIRECTION ( 'NONE',  ( -1.000000000000000000, 1.010728034814421376E-30, 1.090846720500930387E-30 ) ) ;
#9175 = EDGE_LOOP ( 'NONE', ( #559, #1334, #10397 ) ) ;
#9176 = EDGE_CURVE ( 'NONE', #6667, #12656, #596, .T. ) ;
#9177 = ORIENTED_EDGE ( 'NONE', *, *, #9176, .F. ) ;
#9178 = ORIENTED_EDGE ( 'NONE', *, *, #7128, .F. ) ;
#9179 = EDGE_CURVE ( 'NONE', #6636, #9475, #798, .T. ) ;
#9180 = VERTEX_POINT ( 'NONE', #1352 ) ;
#9181 = AXIS2_PLACEMENT_3D ( 'NONE', #7047, #10962, #4015 ) ;
#9182 = CARTESIAN_POINT ( 'NONE',  ( 40.00000000000000711, 14.50364731389636574, -24.59751492040896892 ) ) ;
#9183 = CIRCLE ( 'NONE', #3859, 6.499000000000009436 ) ;
#9184 = CARTESIAN_POINT ( 'NONE',  ( 0.000000000000000000, 0.000000000000000000, 0.000000000000000000 ) ) ;
#9185 = VERTEX_POINT ( 'NONE', #8253 ) ;
#9186 = ADVANCED_FACE ( 'NONE', ( #2273 ), #10103, .F. ) ;
#9187 = DIRECTION ( 'NONE',  ( -1.000000000000000000, 1.010728034814421376E-30, 1.090846720500930387E-30 ) ) ;
#9188 = ORIENTED_EDGE ( 'NONE', *, *, #9075, .T. ) ;
#9189 = DIRECTION ( 'NONE',  ( 0.000000000000000000, 0.000000000000000000, 1.000000000000000000 ) ) ;
#9190 = PRODUCT_DEFINITION_FORMATION_WITH_SPECIFIED_SOURCE ( 'ANY', '', #12041, .NOT_KNOWN. ) ;
#9191 = FACE_OUTER_BOUND ( 'NONE', #4424, .T. ) ;
#9192 = CIRCLE ( 'NONE', #12475, 6.000000000000000888 ) ;
#9193 = AXIS2_PLACEMENT_3D ( 'NONE', #5252, #9233, #9050 ) ;
#9194 = CARTESIAN_POINT ( 'NONE',  ( -37.15000000000005542, 2.632990618166571591E-16, 2.431703406787713260E-15 ) ) ;
#9195 = LINE ( 'NONE', #9131, #11306 ) ;
#9196 = ORIENTED_EDGE ( 'NONE', *, *, #4614, .F. ) ;
#9197 = ORIENTED_EDGE ( 'NONE', *, *, #10999, .T. ) ;
#9198 = CARTESIAN_POINT ( 'NONE',  ( 2.000000000000001776, 0.000000000000000000, 0.000000000000000000 ) ) ;
#9199 = SHAPE_REPRESENTATION ( 'hex flange nut gradea_iso_ISO - 4161 - M5 - N', ( #12422 ), #10082 ) ;
#9200 =( LENGTH_UNIT ( ) NAMED_UNIT ( * ) SI_UNIT ( .MILLI., .METRE. ) );
#9201 = DIRECTION ( 'NONE',  ( 0.000000000000000000, 5.551115123125776539E-17, 1.000000000000000000 ) ) ;
#9202 = DIRECTION ( 'NONE',  ( -1.000000000000000000, 1.010728034814421376E-30, 1.090846720500930387E-30 ) ) ;
#9203 = DIRECTION ( 'NONE',  ( -1.000000000000000000, 1.010728034814421376E-30, 1.090846720500930387E-30 ) ) ;
#9204 = APPLICATION_CONTEXT ( 'automotive_design' ) ;
#9205 = LINE ( 'NONE', #12126, #4827 ) ;
#9206 = DIRECTION ( 'NONE',  ( 1.000000000000000000, -1.010728034814421376E-30, -1.090846720500930387E-30 ) ) ;
#9207 = VERTEX_POINT ( 'NONE', #11153 ) ;
#9208 = LINE ( 'NONE', #4197, #11324 ) ;
#9209 = DIRECTION ( 'NONE',  ( -1.000000000000000000, 1.010728034814421376E-30, 1.090846720500930387E-30 ) ) ;
#9210 = EDGE_LOOP ( 'NONE', ( #3582, #2391, #12417, #2600 ) ) ;
#9211 = DIRECTION ( 'NONE',  ( 0.000000000000000000, 0.000000000000000000, 1.000000000000000000 ) ) ;
#9212 = CARTESIAN_POINT ( 'NONE',  ( 19.99999999999999645, -6.459281472512932609, 1.556709314830556412 ) ) ;
#9213 = CIRCLE ( 'NONE', #3682, 2.000000000000003109 ) ;
#9214 = CARTESIAN_POINT ( 'NONE',  ( -3.999999999999993339, -2.512220745329314830, -3.469390707569731447 ) ) ;
#9215 = CARTESIAN_POINT ( 'NONE',  ( 3.469446951953614189E-15, 4.618802153517009401, -0.5000000000000091038 ) ) ;
#9216 = DIRECTION ( 'NONE',  ( 0.000000000000000000, 1.000000000000000000, 0.000000000000000000 ) ) ;
#9217 = CARTESIAN_POINT ( 'NONE',  ( -15.00000000000000711, -30.00000000000000000, 25.00000000000007105 ) ) ;
#9218 = VERTEX_POINT ( 'NONE', #11022 ) ;
#9219 = DIRECTION ( 'NONE',  ( 2.218671295934093250E-30, -5.551115123125776539E-17, -1.000000000000000000 ) ) ;
#9220 = ORIENTED_EDGE ( 'NONE', *, *, #10392, .T. ) ;
#9221 = AXIS2_PLACEMENT_3D ( 'NONE', #5835, #9748, #941 ) ;
#9222 = VERTEX_POINT ( 'NONE', #2209 ) ;
#9223 = CONTEXT_DEPENDENT_SHAPE_REPRESENTATION ( #3478, #9737 ) ;
#9224 = ORIENTED_EDGE ( 'NONE', *, *, #11193, .F. ) ;
#9225 = EDGE_CURVE ( 'NONE', #12043, #11154, #5226, .T. ) ;
#9226 = DIRECTION ( 'NONE',  ( -0.000000000000000000, 1.530455820933490821E-32, -1.000000000000000000 ) ) ;
#9227 = ADVANCED_FACE ( 'NONE', ( #12192 ), #7293, .T. ) ;
#9228 = CIRCLE ( 'NONE', #11914, 7.400000000000009237 ) ;
#9229 = DIRECTION ( 'NONE',  ( 2.465190328815656418E-32, -1.177425296209236734E-30, -1.000000000000000000 ) ) ;
#9231 = EDGE_CURVE ( 'NONE', #7142, #1792, #456, .T. ) ;
#9230 = CYLINDRICAL_SURFACE ( 'NONE', #8006, 6.499000000000010324 ) ;
#9232 = AXIS2_PLACEMENT_3D ( 'NONE', #5553, #586, #7482 ) ;
#9233 = DIRECTION ( 'NONE',  ( -1.000000000000000000, 1.010728034814421376E-30, 1.090846720500930387E-30 ) ) ;
#9234 = VERTEX_POINT ( 'NONE', #3625 ) ;
#9235 = DIRECTION ( 'NONE',  ( -1.000000000000000000, 1.010728034814421376E-30, 1.090846720500930387E-30 ) ) ;
#9236 = VECTOR ( 'NONE', #2920, 1000.000000000000114 ) ;
#9237 = DIRECTION ( 'NONE',  ( -1.392832535780847392E-30, 0.8345732537213000901, 0.5508969814521065267 ) ) ;
#9238 = ORIENTED_EDGE ( 'NONE', *, *, #3844, .F. ) ;
#9239 = ORIENTED_EDGE ( 'NONE', *, *, #1522, .F. ) ;
#9240 = ORIENTED_EDGE ( 'NONE', *, *, #2202, .F. ) ;
#9241 = AXIS2_PLACEMENT_3D ( 'NONE', #11546, #10555, #11477 ) ;
#9242 = ORIENTED_EDGE ( 'NONE', *, *, #872, .F. ) ;
#9243 = AXIS2_PLACEMENT_3D ( 'NONE', #3254, #8185, #2340 ) ;
#9244 = CIRCLE ( 'NONE', #2277, 1.535500000000001863 ) ;
#9245 = DIRECTION ( 'NONE',  ( -1.000000000000000000, 1.010728034814421376E-30, 1.090846720500930387E-30 ) ) ;
#9246 = DIRECTION ( 'NONE',  ( -1.000000000000000000, 1.010728034814421376E-30, 1.090846720500930387E-30 ) ) ;
#9247 = ORIENTED_EDGE ( 'NONE', *, *, #6194, .T. ) ;
#9248 = DIRECTION ( 'NONE',  ( -1.000000000000000000, 1.010728034814421376E-30, 1.090846720500930387E-30 ) ) ;
#9249 = EDGE_LOOP ( 'NONE', ( #4697, #7573, #1277 ) ) ;
#9250 = CARTESIAN_POINT ( 'NONE',  ( 0.000000000000000000, 4.177097350749788163, 6.108343287861209170 ) ) ;
#9251 = CARTESIAN_POINT ( 'NONE',  ( 19.99999999999999645, 4.192831774278975132, 4.965597920955411304 ) ) ;
#9252 = CIRCLE ( 'NONE', #10896, 6.499000000000008548 ) ;
#9253 = AXIS2_PLACEMENT_3D ( 'NONE', #1093, #9836, #8883 ) ;
#9254 = LINE ( 'NONE', #7341, #6066 ) ;
#9255 = CARTESIAN_POINT ( 'NONE',  ( 11.00000000000001599, 19.99999999999999645, 12.00000000000003020 ) ) ;
#9256 = EDGE_CURVE ( 'NONE', #1582, #5079, #8376, .T. ) ;
#9257 = EDGE_LOOP ( 'NONE', ( #6839, #7715, #2651, #3666 ) ) ;
#9258 = ADVANCED_BREP_SHAPE_REPRESENTATION ( '', ( #10231, #12422 ), #7637 ) ;
#9259 = ORIENTED_EDGE ( 'NONE', *, *, #4283, .T. ) ;
#9260 = CARTESIAN_POINT ( 'NONE',  ( -40.00000000000000000, 30.00000000000000000, 2.000000000000003109 ) ) ;
#9261 =( GEOMETRIC_REPRESENTATION_CONTEXT ( 3 ) GLOBAL_UNCERTAINTY_ASSIGNED_CONTEXT ( ( #1728 ) ) GLOBAL_UNIT_ASSIGNED_CONTEXT ( ( #6656, #9711, #2736 ) ) REPRESENTATION_CONTEXT ( 'NONE', 'WORKASPACE' ) );
#9262 = CARTESIAN_POINT ( 'NONE',  ( -3.999999999999990674, 0.7924765000094612377, -0.05906175389889126159 ) ) ;
#9263 = EDGE_CURVE ( 'NONE', #10485, #3780, #11089, .T. ) ;
#9264 = DIRECTION ( 'NONE',  ( -1.000000000000000000, 0.000000000000000000, 0.000000000000000000 ) ) ;
#9265 = ADVANCED_FACE ( 'NONE', ( #9388 ), #4703, .T. ) ;
#9266 = CARTESIAN_POINT ( 'NONE',  ( 40.00000000000006395, -4.499999999999998224, -20.00000000000000000 ) ) ;
#9267 = CARTESIAN_POINT ( 'NONE',  ( 19.99999999999997868, 6.544726022087268724, 2.140719964816364840 ) ) ;
#9268 = TOROIDAL_SURFACE ( 'NONE', #12182, 4.999999999999997335, 4.000000000000000000 ) ;
#9269 = CARTESIAN_POINT ( 'NONE',  ( 0.000000000000000000, -5.682309657208322484, -3.313524683562052431 ) ) ;
#9270 = ORIENTED_EDGE ( 'NONE', *, *, #1275, .T. ) ;
#9271 = CARTESIAN_POINT ( 'NONE',  ( 0.000000000000000000, 4.618802153516985420, -3.433295621305398893 ) ) ;
#9272 = DIRECTION ( 'NONE',  ( -1.244921116051907679E-30, 0.2660368455666687337, 0.9639628606958550172 ) ) ;
#9273 = AXIS2_PLACEMENT_3D ( 'NONE', #4058, #9139, #12122 ) ;
#9274 = ADVANCED_FACE ( 'NONE', ( #1548 ), #8211, .T. ) ;
#9275 = AXIS2_PLACEMENT_3D ( 'NONE', #6605, #12720, #9596 ) ;
#9276 = ORIENTED_EDGE ( 'NONE', *, *, #8246, .T. ) ;
#9277 = CARTESIAN_POINT ( 'NONE',  ( -30.00000000000000000, -30.00000000000000000, 2.831145448779744488E-15 ) ) ;
#9278 = CARTESIAN_POINT ( 'NONE',  ( 27.00000000000001421, 39.34792583643766761, -19.56347054209567204 ) ) ;
#9279 = CARTESIAN_POINT ( 'NONE',  ( 27.00000000000000355, 14.50364731389636219, -24.59751492040896892 ) ) ;
#9280 = CARTESIAN_POINT ( 'NONE',  ( 4.154306624730794262, -2.398490048084974013, -3.721999068284304713 ) ) ;
#9281 = PLANE ( 'NONE',  #3015 ) ;
#9282 = CARTESIAN_POINT ( 'NONE',  ( 20.00000000000000000, 39.34792583643766051, -17.06347054209567915 ) ) ;
#9283 = ADVANCED_FACE ( 'NONE', ( #2465 ), #5415, .T. ) ;
#9284 = CIRCLE ( 'NONE', #9079, 2.800000000000003819 ) ;
#9285 = VERTEX_POINT ( 'NONE', #4516 ) ;
#9286 = DIRECTION ( 'NONE',  ( -1.000000000000000000, 0.000000000000000000, 2.017120320903271344E-16 ) ) ;
#9287 = VERTEX_POINT ( 'NONE', #5546 ) ;
#9288 = ORIENTED_EDGE ( 'NONE', *, *, #4049, .F. ) ;
#9289 = ORIENTED_EDGE ( 'NONE', *, *, #1789, .F. ) ;
#9290 = CARTESIAN_POINT ( 'NONE',  ( -5.384454397937084025, -2.810041467594755935E-15, -4.484454397937126302 ) ) ;
#9291 = AXIS2_PLACEMENT_3D ( 'NONE', #9198, #1280, #446 ) ;
#9292 = DIRECTION ( 'NONE',  ( 1.000000000000000000, 1.081682119347366197E-16, -6.938893903907228378E-17 ) ) ;
#9293 = CARTESIAN_POINT ( 'NONE',  ( 0.000000000000000000, 30.00000000000000000, 0.000000000000000000 ) ) ;
#9294 = CARTESIAN_POINT ( 'NONE',  ( 19.99999999999999645, 0.000000000000000000, 0.000000000000000000 ) ) ;
#9295 = ORIENTED_EDGE ( 'NONE', *, *, #4598, .F. ) ;
#9296 = CARTESIAN_POINT ( 'NONE',  ( 4.207491450040597769, -2.029819825146486956, -3.671670828759570515 ) ) ;
#9297 = LINE ( 'NONE', #4488, #7010 ) ;
#9298 = VERTEX_POINT ( 'NONE', #3495 ) ;
#9299 = ORIENTED_EDGE ( 'NONE', *, *, #7462, .F. ) ;
#9300 = CIRCLE ( 'NONE', #6446, 2.500000000000000444 ) ;
#9301 = ADVANCED_FACE ( 'NONE', ( #7419 ), #8567, .T. ) ;
#9302 = ORIENTED_EDGE ( 'NONE', *, *, #7782, .T. ) ;
#9303 = AXIS2_PLACEMENT_3D ( 'NONE', #10860, #7784, #8930 ) ;
#9304 = EDGE_CURVE ( 'NONE', #753, #5492, #7598, .T. ) ;
#9305 = ORIENTED_EDGE ( 'NONE', *, *, #4711, .F. ) ;
#9306 = CARTESIAN_POINT ( 'NONE',  ( 14.00000000000000000, 30.00000000000000000, -4.000000000000000000 ) ) ;
#9307 = FACE_BOUND ( 'NONE', #2153, .T. ) ;
#9308 = VERTEX_POINT ( 'NONE', #12386 ) ;
#9309 = CARTESIAN_POINT ( 'NONE',  ( 20.00000000000000000, 0.000000000000000000, 0.000000000000000000 ) ) ;
#9310 = VERTEX_POINT ( 'NONE', #2592 ) ;
#9311 = CIRCLE ( 'NONE', #11797, 0.5155456020628804703 ) ;
#9312 = DIRECTION ( 'NONE',  ( 0.000000000000000000, 0.000000000000000000, -1.000000000000000000 ) ) ;
#9313 = DIRECTION ( 'NONE',  ( 1.000000000000000000, -6.162975822039154730E-33, -4.563833282352349791E-17 ) ) ;
#9314 = DIRECTION ( 'NONE',  ( 7.241496590895994765E-32, 0.6579387259397138088, -0.7530714660036099684 ) ) ;
#9315 = DIRECTION ( 'NONE',  ( 0.000000000000000000, 0.000000000000000000, -1.000000000000000000 ) ) ;
#9316 = EDGE_LOOP ( 'NONE', ( #7576, #5701, #7687, #2080 ) ) ;
#9317 = CIRCLE ( 'NONE', #1515, 6.499000000000006771 ) ;
#9318 = EDGE_CURVE ( 'NONE', #10196, #8613, #6517, .T. ) ;
#9319 = EDGE_LOOP ( 'NONE', ( #6638, #8007, #7886, #7849 ) ) ;
#9320 = CARTESIAN_POINT ( 'NONE',  ( -30.00000000000000000, 0.000000000000000000, 2.000000000000001776 ) ) ;
#9321 = SURFACE_STYLE_USAGE ( .BOTH. , #6184 ) ;
#9322 = FACE_OUTER_BOUND ( 'NONE', #1648, .T. ) ;
#9323 = AXIS2_PLACEMENT_3D ( 'NONE', #5182, #4337, #12012 ) ;
#9324 = CARTESIAN_POINT ( 'NONE',  ( -2.000000000000005329, 3.464101615137750390, 1.561251128379126385E-14 ) ) ;
#9325 = AXIS2_PLACEMENT_3D ( 'NONE', #8999, #11133, #6236 ) ;
#9326 = FACE_OUTER_BOUND ( 'NONE', #1453, .T. ) ;
#9327 = CARTESIAN_POINT ( 'NONE',  ( 21.00000000000003197, 30.00000000000000000, 5.000000000000004441 ) ) ;
#9328 = DIRECTION ( 'NONE',  ( 0.7071067811865504593, 0.000000000000000000, 0.7071067811865445751 ) ) ;
#9329 = ORIENTED_EDGE ( 'NONE', *, *, #6320, .T. ) ;
#9330 = CARTESIAN_POINT ( 'NONE',  ( 3.453038570460582157, 2.625189405341364690, -3.535263753543479659 ) ) ;
#9331 = EDGE_CURVE ( 'NONE', #9308, #412, #707, .T. ) ;
#9332 = AXIS2_PLACEMENT_3D ( 'NONE', #6848, #4501, #4437 ) ;
#9333 = DIRECTION ( 'NONE',  ( -1.000000000000000000, 1.010728034814421376E-30, 1.090846720500930387E-30 ) ) ;
#9334 = EDGE_CURVE ( 'NONE', #8301, #12043, #8000, .T. ) ;
#9335 = CARTESIAN_POINT ( 'NONE',  ( 0.000000000000000000, -4.999339924971583748, 4.274890546383969259 ) ) ;
#9336 = ORIENTED_EDGE ( 'NONE', *, *, #6287, .T. ) ;
#9337 = DIRECTION ( 'NONE',  ( -1.000000000000000000, 1.010728034814421376E-30, 1.090846720500930387E-30 ) ) ;
#9338 = EDGE_CURVE ( 'NONE', #4187, #271, #11528, .T. ) ;
#9339 = DIRECTION ( 'NONE',  ( -1.000000000000000000, 1.010728034814421376E-30, 1.090846720500930387E-30 ) ) ;
#9340 = CARTESIAN_POINT ( 'NONE',  ( 0.000000000000000000, -6.486618105788065414, 0.4009819817179204327 ) ) ;
#9341 = CARTESIAN_POINT ( 'NONE',  ( 3.510273485745297961, 2.827716139362650427, -3.610536846335888228 ) ) ;
#9342 = CIRCLE ( 'NONE', #12651, 2.800000000000003819 ) ;
#9343 = CARTESIAN_POINT ( 'NONE',  ( 40.00000000000000711, 14.39651704831740986, -19.59866274153860388 ) ) ;
#9344 = CARTESIAN_POINT ( 'NONE',  ( 11.17157287525379772, 30.00000000000000000, -2.828427124746177856 ) ) ;
#9345 = SURFACE_STYLE_USAGE ( .BOTH. , #8134 ) ;
#9346 = CARTESIAN_POINT ( 'NONE',  ( -4.154094228333558014, 2.398367420968053221, -3.721909803043253806 ) ) ;
#9347 = VERTEX_POINT ( 'NONE', #522 ) ;
#9348 = AXIS2_PLACEMENT_3D ( 'NONE', #6987, #4860, #8847 ) ;
#9349 = ORIENTED_EDGE ( 'NONE', *, *, #10121, .T. ) ;
#9350 = ORIENTED_EDGE ( 'NONE', *, *, #3381, .F. ) ;
#9351 = DIRECTION ( 'NONE',  ( -1.000000000000000000, 1.010728034814421376E-30, 1.090846720500930387E-30 ) ) ;
#9352 = SURFACE_STYLE_USAGE ( .BOTH. , #8461 ) ;
#9353 = CARTESIAN_POINT ( 'NONE',  ( 0.000000000000000000, -6.577476285968329783, -0.06996125000500660884 ) ) ;
#9354 = CARTESIAN_POINT ( 'NONE',  ( 0.000000000000000000, 1.773042676681338303, 0.000000000000000000 ) ) ;
#9355 = EDGE_LOOP ( 'NONE', ( #11785, #3331, #4083, #12279 ) ) ;
#9356 = CYLINDRICAL_SURFACE ( 'NONE', #10159, 6.499000000000010324 ) ;
#9357 = VECTOR ( 'NONE', #1497, 1000.000000000000000 ) ;
#9358 = LINE ( 'NONE', #7507, #7412 ) ;
#9359 = VERTEX_POINT ( 'NONE', #8499 ) ;
#9360 = ORIENTED_EDGE ( 'NONE', *, *, #1006, .T. ) ;
#9361 = FACE_BOUND ( 'NONE', #1549, .T. ) ;
#9362 = VERTEX_POINT ( 'NONE', #3746 ) ;
#9363 = EDGE_LOOP ( 'NONE', ( #8903, #4420, #1438, #3209 ) ) ;
#9364 = DIRECTION ( 'NONE',  ( -1.140150527077241873E-30, 0.000000000000000000, 1.000000000000000000 ) ) ;
#9365 =( LENGTH_UNIT ( ) NAMED_UNIT ( * ) SI_UNIT ( .MILLI., .METRE. ) );
#9366 = ORIENTED_EDGE ( 'NONE', *, *, #3854, .T. ) ;
#9367 = DIRECTION ( 'NONE',  ( -1.140150527077241873E-30, 0.000000000000000000, 1.000000000000000000 ) ) ;
#9368 = TOROIDAL_SURFACE ( 'NONE', #952, 5.384454397937118664, 0.5155456020628804703 ) ;
#9369 = DIRECTION ( 'NONE',  ( -0.000000000000000000, -1.000000000000000000, -0.000000000000000000 ) ) ;
#9370 = EDGE_LOOP ( 'NONE', ( #10060, #796, #3603, #10906 ) ) ;
#9371 = CYLINDRICAL_SURFACE ( 'NONE', #1800, 2.800000000000003819 ) ;
#9372 = EDGE_CURVE ( 'NONE', #3366, #10769, #12446, .T. ) ;
#9373 = CARTESIAN_POINT ( 'NONE',  ( 0.000000000000000000, -1.623118704078954533, 6.293050665016855838 ) ) ;
#9374 = DIRECTION ( 'NONE',  ( 7.038118388768703491E-30, 0.4999999999999988898, -0.8660254037844392627 ) ) ;
#9375 = DIRECTION ( 'NONE',  ( 1.000000000000000000, -6.162975822039154730E-33, -4.563833282352349791E-17 ) ) ;
#9376 = AXIS2_PLACEMENT_3D ( 'NONE', #4797, #1951, #6731 ) ;
#9377 = EDGE_LOOP ( 'NONE', ( #8596, #10930, #3983, #8222 ) ) ;
#9378 = ORIENTED_EDGE ( 'NONE', *, *, #6612, .F. ) ;
#9379 = DIRECTION ( 'NONE',  ( 0.000000000000000000, -0.2660368455666825005, 0.9639628606958513535 ) ) ;
#9380 = CARTESIAN_POINT ( 'NONE',  ( 6.000000000000000000, 49.63999999999998636, -13.00000000000000178 ) ) ;
#9381 = EDGE_CURVE ( 'NONE', #2497, #1763, #2505, .T. ) ;
#9382 = VECTOR ( 'NONE', #2003, 1000.000000000000114 ) ;
#9383 = CARTESIAN_POINT ( 'NONE',  ( 0.000000000000000000, 0.4528593230174703388, 7.386130139224202473 ) ) ;
#9384 = VECTOR ( 'NONE', #5868, 1000.000000000000000 ) ;
#9385 = EDGE_CURVE ( 'NONE', #4888, #6667, #7202, .T. ) ;
#9386 = EDGE_CURVE ( 'NONE', #11644, #5515, #8831, .T. ) ;
#9387 = DIRECTION ( 'NONE',  ( 0.000000000000000000, 0.000000000000000000, 1.000000000000000000 ) ) ;
#9388 = FACE_OUTER_BOUND ( 'NONE', #8332, .T. ) ;
#9389 = EDGE_LOOP ( 'NONE', ( #10512, #8860, #8283, #4084, #10080, #5826 ) ) ;
#9390 = LINE ( 'NONE', #8570, #7205 ) ;
#9391 = DIRECTION ( 'NONE',  ( 0.000000000000000000, 0.000000000000000000, 1.000000000000000000 ) ) ;
#9392 = CARTESIAN_POINT ( 'NONE',  ( 33.00000000000001421, 81.84122341717352356, -42.68198508464162444 ) ) ;
#9393 = VERTEX_POINT ( 'NONE', #12575 ) ;
#9394 = ADVANCED_FACE ( 'NONE', ( #4647 ), #3680, .T. ) ;
#9395 = CYLINDRICAL_SURFACE ( 'NONE', #8890, 2.800000000000003819 ) ;
#9396 = LINE ( 'NONE', #8191, #5012 ) ;
#9397 = DIRECTION ( 'NONE',  ( -1.000000000000000000, 1.010728034814421376E-30, 1.090846720500930387E-30 ) ) ;
#9398 = EDGE_CURVE ( 'NONE', #11114, #3023, #1926, .T. ) ;
#9399 = DIRECTION ( 'NONE',  ( 1.000000000000000000, -1.010728034814421376E-30, -1.090846720500930387E-30 ) ) ;
#9400 = LINE ( 'NONE', #6465, #934 ) ;
#9401 = EDGE_CURVE ( 'NONE', #3832, #11920, #1804, .T. ) ;
#9402 = CARTESIAN_POINT ( 'NONE',  ( -30.00000000000000000, 0.000000000000000000, 2.185182530847200403E-15 ) ) ;
#9403 = ADVANCED_FACE ( 'NONE', ( #9768 ), #834, .F. ) ;
#9404 = CARTESIAN_POINT ( 'NONE',  ( 14.00000000000000000, 44.64000000000000057, -5.000000000000000888 ) ) ;
#9405 = EDGE_LOOP ( 'NONE', ( #12037, #8202, #8544, #6408 ) ) ;
#9406 = AXIS2_PLACEMENT_3D ( 'NONE', #8722, #5755, #7875 ) ;
#9407 = VERTEX_POINT ( 'NONE', #1023 ) ;
#9408 = VERTEX_POINT ( 'NONE', #5729 ) ;
#9409 = CARTESIAN_POINT ( 'NONE',  ( 20.00000000000000000, 39.34792583643766051, -14.91347054209568945 ) ) ;
#9410 = CARTESIAN_POINT ( 'NONE',  ( 20.00000000000000000, 16.67945018363952059, -6.690790236289298143 ) ) ;
#9411 = CARTESIAN_POINT ( 'NONE',  ( -15.00000000000000000, -19.99999999999998934, 12.00000000000002842 ) ) ;
#9412 = ADVANCED_FACE ( 'NONE', ( #1 ), #8878, .F. ) ;
#9413 = DIRECTION ( 'NONE',  ( 0.000000000000000000, 0.000000000000000000, -1.000000000000000000 ) ) ;
#9414 = ORIENTED_EDGE ( 'NONE', *, *, #11800, .F. ) ;
#9415 = EDGE_CURVE ( 'NONE', #5515, #4888, #7735, .T. ) ;
#9416 = DIRECTION ( 'NONE',  ( 0.000000000000000000, 0.000000000000000000, 1.000000000000000000 ) ) ;
#9417 = VECTOR ( 'NONE', #12024, 1000.000000000000000 ) ;
#9418 = DIRECTION ( 'NONE',  ( -1.000000000000000000, 1.010728034814421376E-30, 1.090846720500930387E-30 ) ) ;
#9419 = ORIENTED_EDGE ( 'NONE', *, *, #576, .T. ) ;
#9420 = EDGE_LOOP ( 'NONE', ( #12085, #1313, #12036, #1140 ) ) ;
#9421 = CARTESIAN_POINT ( 'NONE',  ( 9.000000000000028422, 30.00000000000000000, 1.387778780781438526E-16 ) ) ;
#9422 = ORIENTED_EDGE ( 'NONE', *, *, #9569, .F. ) ;
#9423 = ORIENTED_EDGE ( 'NONE', *, *, #3685, .T. ) ;
#9424 = DIRECTION ( 'NONE',  ( 0.000000000000000000, 0.000000000000000000, -1.000000000000000000 ) ) ;
#9425 = VECTOR ( 'NONE', #2731, 1000.000000000000000 ) ;
#9426 = VECTOR ( 'NONE', #8623, 1000.000000000000114 ) ;
#9427 = CIRCLE ( 'NONE', #3897, 9.999999999999998224 ) ;
#9428 = ORIENTED_EDGE ( 'NONE', *, *, #6267, .T. ) ;
#9429 = FACE_OUTER_BOUND ( 'NONE', #3227, .T. ) ;
#9430 = DIRECTION ( 'NONE',  ( -1.000000000000000000, -5.916456789157575403E-31, 1.577021341797099039E-16 ) ) ;
#9431 = VECTOR ( 'NONE', #2960, 1000.000000000000000 ) ;
#9432 = ORIENTED_EDGE ( 'NONE', *, *, #2550, .F. ) ;
#9433 = CARTESIAN_POINT ( 'NONE',  ( 9.000000000000028422, -30.00000000000000000, 5.000000000000011546 ) ) ;
#9434 = CARTESIAN_POINT ( 'NONE',  ( 21.00000000000004974, -12.49999999999999289, 5.000000000000007994 ) ) ;
#9435 = ADVANCED_FACE ( 'NONE', ( #10807 ), #607, .T. ) ;
#9436 = CARTESIAN_POINT ( 'NONE',  ( 20.00000000000000000, 16.67945018363952059, -6.690790236289298143 ) ) ;
#9437 = CIRCLE ( 'NONE', #11721, 4.000000000000001776 ) ;
#9438 = UNCERTAINTY_MEASURE_WITH_UNIT (LENGTH_MEASURE( 1.000000000000000082E-05 ), #4457, 'distance_accuracy_value', 'NONE');
#9439 = CIRCLE ( 'NONE', #7809, 7.400000000000009237 ) ;
#9440 = DIRECTION ( 'NONE',  ( 1.140150527077241873E-30, 0.000000000000000000, -1.000000000000000000 ) ) ;
#9441 = EDGE_CURVE ( 'NONE', #9126, #8587, #12559, .T. ) ;
#9442 = ORIENTED_EDGE ( 'NONE', *, *, #11707, .F. ) ;
#9443 = EDGE_LOOP ( 'NONE', ( #1200, #10827, #12435, #4574 ) ) ;
#9444 = CARTESIAN_POINT ( 'NONE',  ( 9.999999999999998224, 4.177097350749886751, -6.108343287861160320 ) ) ;
#9445 = DIRECTION ( 'NONE',  ( 0.000000000000000000, 0.000000000000000000, 1.000000000000000000 ) ) ;
#9446 = ORIENTED_EDGE ( 'NONE', *, *, #1349, .F. ) ;
#9447 = CARTESIAN_POINT ( 'NONE',  ( 40.00000000000000000, 39.49790820824818383, -24.06186359251417883 ) ) ;
#9448 = MECHANICAL_DESIGN_GEOMETRIC_PRESENTATION_REPRESENTATION (  '', ( #12153 ), #11111 ) ;
#9449 = AXIS2_PLACEMENT_3D ( 'NONE', #6526, #8382, #10501 ) ;
#9450 = DIRECTION ( 'NONE',  ( -1.000000000000000000, 1.010728034814421376E-30, 1.090846720500930387E-30 ) ) ;
#9451 = ADVANCED_FACE ( 'NONE', ( #5023 ), #12700, .T. ) ;
#9452 = DIRECTION ( 'NONE',  ( 1.000000000000000000, -0.000000000000000000, -6.938893903907228378E-17 ) ) ;
#9453 = CARTESIAN_POINT ( 'NONE',  ( 19.99999999999997868, 5.895746314278407674, -2.916892913127022702 ) ) ;
#9454 = VERTEX_POINT ( 'NONE', #2859 ) ;
#9455 = FACE_OUTER_BOUND ( 'NONE', #5395, .T. ) ;
#9456 = AXIS2_PLACEMENT_3D ( 'NONE', #4019, #3139, #2951 ) ;
#9457 = DIRECTION ( 'NONE',  ( -1.000000000000000000, 1.010728034814421376E-30, 1.090846720500930387E-30 ) ) ;
#9458 = EDGE_CURVE ( 'NONE', #7454, #10609, #1019, .T. ) ;
#9459 = ADVANCED_FACE ( 'NONE', ( #7909 ), #959, .T. ) ;
#9460 = ADVANCED_FACE ( 'NONE', ( #11600 ), #8638, .F. ) ;
#9461 = FACE_OUTER_BOUND ( 'NONE', #1142, .T. ) ;
#9462 = ORIENTED_EDGE ( 'NONE', *, *, #8855, .T. ) ;
#9463 = DIRECTION ( 'NONE',  ( 0.000000000000000000, 0.3513748240813434620, -0.9362348706397368714 ) ) ;
#9464 = CARTESIAN_POINT ( 'NONE',  ( -2.000000000000005329, 3.464101615137750390, 1.561251128379126385E-14 ) ) ;
#9465 = DIRECTION ( 'NONE',  ( -1.848892746611746419E-31, -1.000000000000000000, 3.250006781153460502E-32 ) ) ;
#9466 = DIRECTION ( 'NONE',  ( -1.000000000000000000, -1.081682119347366197E-16, 6.938893903907228378E-17 ) ) ;
#9467 = CARTESIAN_POINT ( 'NONE',  ( 14.00000000000000000, 44.64000000000000057, -6.938893903907228378E-15 ) ) ;
#9468 = DIRECTION ( 'NONE',  ( -1.000000000000000000, 1.010728034814421376E-30, 1.090846720500930387E-30 ) ) ;
#9469 = SURFACE_STYLE_USAGE ( .BOTH. , #8652 ) ;
#9470 = CARTESIAN_POINT ( 'NONE',  ( 19.99999999999997868, -0.1095571986794155184, -6.498076501567039642 ) ) ;
#9471 = VERTEX_POINT ( 'NONE', #4772 ) ;
#9472 = VECTOR ( 'NONE', #2815, 1000.000000000000000 ) ;
#9473 = EDGE_CURVE ( 'NONE', #8922, #444, #6768, .T. ) ;
#9474 = ORIENTED_EDGE ( 'NONE', *, *, #6721, .F. ) ;
#9475 = VERTEX_POINT ( 'NONE', #3046 ) ;
#9476 = DIRECTION ( 'NONE',  ( -1.000000000000000000, 1.010728034814421376E-30, 1.090846720500930387E-30 ) ) ;
#9477 = CARTESIAN_POINT ( 'NONE',  ( 19.99999999999999645, -4.999339924971576643, 4.274890546383965706 ) ) ;
#9478 = AXIS2_PLACEMENT_3D ( 'NONE', #2657, #11344, #10426 ) ;
#9479 = CARTESIAN_POINT ( 'NONE',  ( 0.000000000000000000, 4.862606272033057841, -3.745885042887454830 ) ) ;
#9480 = ORIENTED_EDGE ( 'NONE', *, *, #10351, .T. ) ;
#9481 = EDGE_CURVE ( 'NONE', #12721, #7775, #8696, .T. ) ;
#9482 = DIRECTION ( 'NONE',  ( -1.000000000000000000, 1.010728034814421376E-30, 1.090846720500930387E-30 ) ) ;
#9483 = VECTOR ( 'NONE', #9521, 1000.000000000000000 ) ;
#9484 = EDGE_CURVE ( 'NONE', #8975, #9071, #7808, .T. ) ;
#9485 = CARTESIAN_POINT ( 'NONE',  ( 19.99999999999999645, 0.6915992404089836842, 6.462096524400245734 ) ) ;
#9486 = ORIENTED_EDGE ( 'NONE', *, *, #4068, .T. ) ;
#9487 = ORIENTED_EDGE ( 'NONE', *, *, #1716, .T. ) ;
#9488 = DIRECTION ( 'NONE',  ( 1.000000000000000000, 1.849040895279789667E-31, -6.938893903907224680E-17 ) ) ;
#9489 = VERTEX_POINT ( 'NONE', #4051 ) ;
#9490 = ORIENTED_EDGE ( 'NONE', *, *, #5283, .T. ) ;
#9491 = EDGE_CURVE ( 'NONE', #7331, #10149, #4522, .T. ) ;
#9492 = CIRCLE ( 'NONE', #9291, 1.535500000000000087 ) ;
#9493 = EDGE_CURVE ( 'NONE', #1407, #3366, #11008, .T. ) ;
#9494 = LINE ( 'NONE', #8353, #7530 ) ;
#9495 = EDGE_LOOP ( 'NONE', ( #2097, #3, #4763, #12018 ) ) ;
#9496 = EDGE_CURVE ( 'NONE', #5504, #3477, #7024, .T. ) ;
#9497 = DIRECTION ( 'NONE',  ( 0.000000000000000000, -0.8660254037844390407, -0.4999999999999992784 ) ) ;
#9498 = DIRECTION ( 'NONE',  ( -1.159061634649218351E-16, 0.000000000000000000, -1.000000000000000000 ) ) ;
#9499 = ORIENTED_EDGE ( 'NONE', *, *, #12666, .T. ) ;
#9500 = CARTESIAN_POINT ( 'NONE',  ( 19.99999999999997868, -0.1095571986794155184, -6.498076501567039642 ) ) ;
#9501 = EDGE_CURVE ( 'NONE', #3728, #6024, #10212, .T. ) ;
#9502 = DIRECTION ( 'NONE',  ( 0.000000000000000000, 0.000000000000000000, 1.000000000000000000 ) ) ;
#9503 = AXIS2_PLACEMENT_3D ( 'NONE', #3384, #6069, #9211 ) ;
#9504 = DIRECTION ( 'NONE',  ( 0.000000000000000000, 0.7818314824680310249, -0.6234898018587319291 ) ) ;
#9505 = CIRCLE ( 'NONE', #10543, 6.499000000000009436 ) ;
#9506 = ORIENTED_EDGE ( 'NONE', *, *, #3391, .T. ) ;
#9507 = ORIENTED_EDGE ( 'NONE', *, *, #687, .F. ) ;
#9508 = DIRECTION ( 'NONE',  ( 0.000000000000000000, -0.000000000000000000, 1.000000000000000000 ) ) ;
#9509 = AXIS2_PLACEMENT_3D ( 'NONE', #12280, #8460, #5508 ) ;
#9510 = CARTESIAN_POINT ( 'NONE',  ( 0.000000000000000000, 0.000000000000000000, 0.000000000000000000 ) ) ;
#9511 = ORIENTED_EDGE ( 'NONE', *, *, #3273, .T. ) ;
#9512 = CARTESIAN_POINT ( 'NONE',  ( 9.999999999999998224, 1.764426149628241625, -7.186570834724189005 ) ) ;
#9513 = DIRECTION ( 'NONE',  ( 0.000000000000000000, 0.000000000000000000, -1.000000000000000000 ) ) ;
#9514 = EDGE_CURVE ( 'NONE', #7720, #1057, #9636, .T. ) ;
#9515 = DIRECTION ( 'NONE',  ( 1.000000000000000000, 0.000000000000000000, 0.000000000000000000 ) ) ;
#9516 = AXIS2_PLACEMENT_3D ( 'NONE', #7171, #8962, #2216 ) ;
#9517 = DIRECTION ( 'NONE',  ( -1.848892746611746419E-31, -1.000000000000000000, 3.250006781153460502E-32 ) ) ;
#9518 = VERTEX_POINT ( 'NONE', #8239 ) ;
#9519 = CARTESIAN_POINT ( 'NONE',  ( 20.00000000000000355, 8.524480291341568261, -16.78569157243880383 ) ) ;
#9520 = VERTEX_POINT ( 'NONE', #6177 ) ;
#9521 = DIRECTION ( 'NONE',  ( -1.000000000000000000, 1.010728034814421376E-30, 1.090846720500930387E-30 ) ) ;
#9522 = DIRECTION ( 'NONE',  ( 1.140150527077241873E-30, 0.000000000000000000, -1.000000000000000000 ) ) ;
#9523 = CIRCLE ( 'NONE', #11194, 2.800000000000002931 ) ;
#9524 = CARTESIAN_POINT ( 'NONE',  ( 2.000000000000001776, 1.329782007511007169, -0.7677499999999976010 ) ) ;
#9525 = CARTESIAN_POINT ( 'NONE',  ( 19.99999999999997868, -0.4733669331951446679, -6.481737787550303942 ) ) ;
#9526 = PRODUCT_DEFINITION_SHAPE ( 'NONE', 'NONE',  #12752 ) ;
#9527 = DIRECTION ( 'NONE',  ( 0.000000000000000000, 0.000000000000000000, 1.000000000000000000 ) ) ;
#9528 = DIRECTION ( 'NONE',  ( -1.000000000000000000, 0.000000000000000000, 1.159061634649218351E-16 ) ) ;
#9529 = ADVANCED_FACE ( 'NONE', ( #1276 ), #7220, .T. ) ;
#9530 = CARTESIAN_POINT ( 'NONE',  ( 9.999999999999998224, 12.99999999999999822, -6.123233995736765296E-16 ) ) ;
#9531 = EDGE_CURVE ( 'NONE', #2884, #2783, #1405, .T. ) ;
#9532 = DIRECTION ( 'NONE',  ( 0.000000000000000000, 0.08963930890342669544, 0.9959742939952396235 ) ) ;
#9533 = SURFACE_STYLE_FILL_AREA ( #5565 ) ;
#9534 = UNCERTAINTY_MEASURE_WITH_UNIT (LENGTH_MEASURE( 1.000000000000000082E-05 ), #1882, 'distance_accuracy_value', 'NONE');
#9535 = DIRECTION ( 'NONE',  ( -1.000000000000000000, -1.031065855027150586E-29, 2.218671295934095703E-30 ) ) ;
#9536 = ORIENTED_EDGE ( 'NONE', *, *, #5183, .T. ) ;
#9537 = ORIENTED_EDGE ( 'NONE', *, *, #10288, .T. ) ;
#9538 = VECTOR ( 'NONE', #7778, 1000.000000000000000 ) ;
#9539 = EDGE_LOOP ( 'NONE', ( #1793, #10666, #12009 ) ) ;
#9540 = DIRECTION ( 'NONE',  ( 0.000000000000000000, 1.000000000000000000, -1.467581828789149335E-15 ) ) ;
#9541 = CARTESIAN_POINT ( 'NONE',  ( 19.99999999999999645, -0.1095571986795048497, 6.498076501567022767 ) ) ;
#9542 = CYLINDRICAL_SURFACE ( 'NONE', #10662, 2.800000000000003819 ) ;
#9543 = DIRECTION ( 'NONE',  ( 1.000000000000000000, 1.031065855027150586E-29, -2.218671295934095703E-30 ) ) ;
#9544 = ORIENTED_EDGE ( 'NONE', *, *, #3145, .T. ) ;
#9545 = CARTESIAN_POINT ( 'NONE',  ( 0.000000000000000000, 1.773042676681341856, -3.469446951953614189E-15 ) ) ;
#9546 = EDGE_CURVE ( 'NONE', #9359, #4665, #4733, .T. ) ;
#9547 = PRODUCT_RELATED_PRODUCT_CATEGORY ( 'part', '', ( #8328 ) ) ;
#9548 =( NAMED_UNIT ( * ) SI_UNIT ( $, .STERADIAN. ) SOLID_ANGLE_UNIT ( ) );
#9549 = ORIENTED_EDGE ( 'NONE', *, *, #8296, .F. ) ;
#9550 = VECTOR ( 'NONE', #10587, 1000.000000000000000 ) ;
#9551 = VERTEX_POINT ( 'NONE', #3302 ) ;
#9552 = FACE_OUTER_BOUND ( 'NONE', #365, .T. ) ;
#9553 = ORIENTED_EDGE ( 'NONE', *, *, #1195, .F. ) ;
#9554 = ORIENTED_EDGE ( 'NONE', *, *, #2739, .T. ) ;
#9555 = CARTESIAN_POINT ( 'NONE',  ( 0.000000000000000000, 0.000000000000000000, 0.000000000000000000 ) ) ;
#9556 = PRODUCT_DEFINITION_SHAPE ( 'NONE', 'NONE',  #12751 ) ;
#9557 = CARTESIAN_POINT ( 'NONE',  ( 40.00000000000000711, 11.10553687445043280, -10.07215277424223032 ) ) ;
#9558 = VERTEX_POINT ( 'NONE', #5273 ) ;
#9559 = DIRECTION ( 'NONE',  ( 0.000000000000000000, 0.4999999999999992784, -0.8660254037844390407 ) ) ;
#9560 = CARTESIAN_POINT ( 'NONE',  ( 14.00000000000000000, 30.00000000000000000, -4.000000000000000000 ) ) ;
#9561 = ORIENTED_EDGE ( 'NONE', *, *, #8517, .T. ) ;
#9562 = LINE ( 'NONE', #7400, #2559 ) ;
#9563 = DIRECTION ( 'NONE',  ( 0.000000000000000000, 0.000000000000000000, -1.000000000000000000 ) ) ;
#9564 = ADVANCED_FACE ( 'NONE', ( #188 ), #8037, .F. ) ;
#9565 = EDGE_CURVE ( 'NONE', #12421, #2328, #5961, .T. ) ;
#9566 = VERTEX_POINT ( 'NONE', #11139 ) ;
#9567 = ORIENTED_EDGE ( 'NONE', *, *, #8352, .T. ) ;
#9568 = LINE ( 'NONE', #10486, #5807 ) ;
#9569 = EDGE_CURVE ( 'NONE', #2770, #6747, #3103, .T. ) ;
#9570 = VECTOR ( 'NONE', #3219, 1000.000000000000000 ) ;
#9571 = DIRECTION ( 'NONE',  ( 1.000000000000000000, 0.000000000000000000, 0.000000000000000000 ) ) ;
#9572 = ORIENTED_EDGE ( 'NONE', *, *, #8248, .F. ) ;
#9573 = DIRECTION ( 'NONE',  ( 0.000000000000000000, 0.000000000000000000, 1.000000000000000000 ) ) ;
#9574 = CARTESIAN_POINT ( 'NONE',  ( 2.000000000000001776, 1.773042676681338303, 0.000000000000000000 ) ) ;
#9575 = CIRCLE ( 'NONE', #1160, 2.800000000000002931 ) ;
#9576 = AXIS2_PLACEMENT_3D ( 'NONE', #5692, #11438, #4734 ) ;
#9577 = CARTESIAN_POINT ( 'NONE',  ( 19.99999999999999645, -4.621065432155044839, -4.569765340993108715 ) ) ;
#9578 = CARTESIAN_POINT ( 'NONE',  ( 2.000000000000091926, -0.8865213383406727043, -1.535499999999998755 ) ) ;
#9579 = VERTEX_POINT ( 'NONE', #8101 ) ;
#9580 = DIRECTION ( 'NONE',  ( -1.140150527077241873E-30, 0.000000000000000000, 1.000000000000000000 ) ) ;
#9581 = ORIENTED_EDGE ( 'NONE', *, *, #2028, .T. ) ;
#9582 = CARTESIAN_POINT ( 'NONE',  ( -4.024497503033700241, -2.323544716729510018, -3.572167766733751915 ) ) ;
#9583 = VERTEX_POINT ( 'NONE', #2772 ) ;
#9584 = SURFACE_STYLE_USAGE ( .BOTH. , #12581 ) ;
#9585 = CIRCLE ( 'NONE', #11258, 7.400000000000011902 ) ;
#9586 = AXIS2_PLACEMENT_3D ( 'NONE', #7429, #10506, #3633 ) ;
#9587 = DIRECTION ( 'NONE',  ( 1.000000000000000000, -1.010728034814421376E-30, -1.090846720500930387E-30 ) ) ;
#9588 = CYLINDRICAL_SURFACE ( 'NONE', #5378, 2.800000000000003819 ) ;
#9589 = CARTESIAN_POINT ( 'NONE',  ( 0.000000000000000000, 5.362412286431451847, 3.809543717993933765 ) ) ;
#9590 = DIRECTION ( 'NONE',  ( 0.000000000000000000, 0.000000000000000000, -1.000000000000000000 ) ) ;
#9591 = DIRECTION ( 'NONE',  ( 0.000000000000000000, 0.000000000000000000, 1.000000000000000000 ) ) ;
#9592 = DIRECTION ( 'NONE',  ( 0.000000000000000000, 0.000000000000000000, -1.000000000000000000 ) ) ;
#9593 = LINE ( 'NONE', #11615, #10770 ) ;
#9594 = CIRCLE ( 'NONE', #4681, 6.499000000000005883 ) ;
#9595 = EDGE_CURVE ( 'NONE', #10909, #11856, #249, .T. ) ;
#9596 = DIRECTION ( 'NONE',  ( 0.000000000000000000, 0.000000000000000000, 1.000000000000000000 ) ) ;
#9597 = ORIENTED_EDGE ( 'NONE', *, *, #5150, .T. ) ;
#9598 = EDGE_LOOP ( 'NONE', ( #11798, #12441, #362, #5330 ) ) ;
#9599 = ORIENTED_EDGE ( 'NONE', *, *, #5538, .T. ) ;
#9600 = LINE ( 'NONE', #858, #4605 ) ;
#9601 = CARTESIAN_POINT ( 'NONE',  ( 20.00000000000000355, 19.99999999999999645, -14.14999999999999325 ) ) ;
#9602 = CARTESIAN_POINT ( 'NONE',  ( 33.00000000000001421, 39.49790820824818383, -24.06186359251418594 ) ) ;
#9603 = DIRECTION ( 'NONE',  ( 1.368180632492690949E-30, -0.8805955318567323387, -0.4738686624730092944 ) ) ;
#9604 = ORIENTED_EDGE ( 'NONE', *, *, #6220, .T. ) ;
#9605 = DIRECTION ( 'NONE',  ( 0.000000000000000000, 0.000000000000000000, 1.000000000000000000 ) ) ;
#9606 =( REPRESENTATION_RELATIONSHIP ('NONE','NONE', #10018, #10094 ) REPRESENTATION_RELATIONSHIP_WITH_TRANSFORMATION ( #2297 )SHAPE_REPRESENTATION_RELATIONSHIP( ) );
#9607 = DIRECTION ( 'NONE',  ( 0.000000000000000000, 0.000000000000000000, 1.000000000000000000 ) ) ;
#9608 = EDGE_LOOP ( 'NONE', ( #11171, #11949, #8163, #7827 ) ) ;
#9609 = ORIENTED_EDGE ( 'NONE', *, *, #6633, .T. ) ;
#9610 = CARTESIAN_POINT ( 'NONE',  ( 14.00000000000000000, 49.63999999999998636, -5.000000000000001776 ) ) ;
#9611 = VERTEX_POINT ( 'NONE', #10088 ) ;
#9612 = VECTOR ( 'NONE', #10551, 1000.000000000000000 ) ;
#9613 = ORIENTED_EDGE ( 'NONE', *, *, #360, .F. ) ;
#9614 = EDGE_CURVE ( 'NONE', #6684, #10144, #9195, .T. ) ;
#9615 = ADVANCED_FACE ( 'NONE', ( #10022 ), #3907, .F. ) ;
#9616 = CARTESIAN_POINT ( 'NONE',  ( 9.999999999999998224, -5.492355906873347848, -4.959236492872019397 ) ) ;
#9617 = ADVANCED_FACE ( 'NONE', ( #2389 ), #5339, .F. ) ;
#9618 = ORIENTED_EDGE ( 'NONE', *, *, #4984, .F. ) ;
#9619 = CARTESIAN_POINT ( 'NONE',  ( 6.000000000000000000, 49.63999999999998636, -13.00000000000000178 ) ) ;
#9620 = CARTESIAN_POINT ( 'NONE',  ( 11.00000000000001599, -12.49999999999999645, -4.423544863740860615E-14 ) ) ;
#9621 = ORIENTED_EDGE ( 'NONE', *, *, #2514, .T. ) ;
#9622 = DIRECTION ( 'NONE',  ( 0.000000000000000000, 0.9989930665413145894, 0.04486483035051865020 ) ) ;
#9623 = LINE ( 'NONE', #5592, #8522 ) ;
#9624 = CIRCLE ( 'NONE', #11910, 2.149999999999994138 ) ;
#9625 = ORIENTED_EDGE ( 'NONE', *, *, #9001, .T. ) ;
#9626 = VERTEX_POINT ( 'NONE', #11071 ) ;
#9627 = AXIS2_PLACEMENT_3D ( 'NONE', #11808, #3057, #3881 ) ;
#9628 = VECTOR ( 'NONE', #12235, 1000.000000000000000 ) ;
#9629 = EDGE_LOOP ( 'NONE', ( #5200, #10671 ) ) ;
#9630 = CARTESIAN_POINT ( 'NONE',  ( -37.15000000000006253, 2.632990618166587368E-16, 2.000000000000002220 ) ) ;
#9631 = STYLED_ITEM ( 'NONE', ( #3971 ), #1664 ) ;
#9632 = CARTESIAN_POINT ( 'NONE',  ( 13.00000000000000178, 3.685944058581980235E-14, -20.00000000000014211 ) ) ;
#9633 = EDGE_LOOP ( 'NONE', ( #8972, #7702, #5586, #2928, #9480 ) ) ;
#9634 = DIRECTION ( 'NONE',  ( -0.5000000000000019984, -0.8660254037844375974, -2.465190328815657787E-32 ) ) ;
#9635 = CARTESIAN_POINT ( 'NONE',  ( 40.00000000000000711, 19.99999999999999645, -12.00000000000000178 ) ) ;
#9636 = CIRCLE ( 'NONE', #10675, 2.000000000000003109 ) ;
#9637 = CIRCLE ( 'NONE', #2268, 2.800000000000003819 ) ;
#9638 = EDGE_CURVE ( 'NONE', #11818, #9185, #9437, .T. ) ;
#9639 = CARTESIAN_POINT ( 'NONE',  ( 14.00000000000000000, 30.00000000000000000, 0.000000000000000000 ) ) ;
#9640 = AXIS2_PLACEMENT_3D ( 'NONE', #11055, #8148, #8277 ) ;
#9641 = DIRECTION ( 'NONE',  ( 0.8660254037844379305, 0.5000000000000013323, 0.000000000000000000 ) ) ;
#9642 = EDGE_CURVE ( 'NONE', #6291, #4508, #6162, .T. ) ;
#9643 = ORIENTED_EDGE ( 'NONE', *, *, #2776, .F. ) ;
#9644 = DIRECTION ( 'NONE',  ( -0.000000000000000000, -1.000000000000000000, -0.000000000000000000 ) ) ;
#9645 = VERTEX_POINT ( 'NONE', #1152 ) ;
#9646 = CARTESIAN_POINT ( 'NONE',  ( 0.000000000000000000, -6.577476285968329783, -0.06996125000500660884 ) ) ;
#9647 = CIRCLE ( 'NONE', #3720, 7.400000000000009237 ) ;
#9648 = CIRCLE ( 'NONE', #11529, 2.100000000000000089 ) ;
#9649 = VECTOR ( 'NONE', #3874, 1000.000000000000000 ) ;
#9650 = EDGE_CURVE ( 'NONE', #5440, #937, #508, .T. ) ;
#9651 = EDGE_CURVE ( 'NONE', #2754, #1206, #8433, .T. ) ;
#9652 = DIRECTION ( 'NONE',  ( -1.000000000000000000, 1.010728034814421376E-30, 1.090846720500930387E-30 ) ) ;
#9653 = CARTESIAN_POINT ( 'NONE',  ( 9.757359312880696578, -30.00000000000000000, -4.242640687119267007 ) ) ;
#9654 = CARTESIAN_POINT ( 'NONE',  ( 0.000000000000000000, 0.000000000000000000, 0.000000000000000000 ) ) ;
#9655 = LINE ( 'NONE', #2002, #1588 ) ;
#9656 = CARTESIAN_POINT ( 'NONE',  ( 0.3461262719736449833, -4.658553426539310038, -3.671615880910380270 ) ) ;
#9657 = CARTESIAN_POINT ( 'NONE',  ( 9.999999999999994671, -6.289597356626455138, -3.898841506334599138 ) ) ;
#9658 = VECTOR ( 'NONE', #5056, 1000.000000000000000 ) ;
#9659 = FACE_OUTER_BOUND ( 'NONE', #7704, .T. ) ;
#9660 = FACE_OUTER_BOUND ( 'NONE', #1297, .T. ) ;
#9661 = PRODUCT_DEFINITION_CONTEXT ( 'detailed design', #3061, 'design' ) ;
#9662 = CARTESIAN_POINT ( 'NONE',  ( -4.000000000000012434, 2.309401076758501592, -3.433295621305395340 ) ) ;
#9663 = VERTEX_POINT ( 'NONE', #5531 ) ;
#9664 = ORIENTED_EDGE ( 'NONE', *, *, #8242, .T. ) ;
#9665 = CARTESIAN_POINT ( 'NONE',  ( 2.000000000000010214, -3.464101615137749945, -3.142992957459262549 ) ) ;
#9666 = CARTESIAN_POINT ( 'NONE',  ( 4.000000000000000000, -0.3979232138631230709, -2.371692252312040025E-17 ) ) ;
#9667 = CARTESIAN_POINT ( 'NONE',  ( 2.000000000000001776, -0.8865213383406691516, 1.535500000000002085 ) ) ;
#9668 = CARTESIAN_POINT ( 'NONE',  ( 0.000000000000000000, -5.610543508060412243, -3.433640984893328252 ) ) ;
#9669 = ORIENTED_EDGE ( 'NONE', *, *, #10502, .T. ) ;
#9670 = EDGE_CURVE ( 'NONE', #4184, #12673, #12571, .T. ) ;
#9671 = CARTESIAN_POINT ( 'NONE',  ( 4.197393957002303999, 0.8151795401431323196, -3.503767560748939580 ) ) ;
#9672 = AXIS2_PLACEMENT_3D ( 'NONE', #9100, #12080, #10122 ) ;
#9673 = SURFACE_STYLE_FILL_AREA ( #2890 ) ;
#9674 = ORIENTED_EDGE ( 'NONE', *, *, #5441, .F. ) ;
#9675 = ORIENTED_EDGE ( 'NONE', *, *, #12697, .F. ) ;
#9676 = CARTESIAN_POINT ( 'NONE',  ( 20.00000000000000000, 22.56100271565320625, -6.249672610153678143 ) ) ;
#9677 = ORIENTED_EDGE ( 'NONE', *, *, #10773, .T. ) ;
#9678 = EDGE_LOOP ( 'NONE', ( #6067, #8966, #12407, #2361, #12683 ) ) ;
#9679 =( NAMED_UNIT ( * ) SI_UNIT ( $, .STERADIAN. ) SOLID_ANGLE_UNIT ( ) );
#9680 = CARTESIAN_POINT ( 'NONE',  ( 0.000000000000000000, 4.618802153516985420, -3.433295621305398893 ) ) ;
#9681 = VERTEX_POINT ( 'NONE', #2450 ) ;
#9682 = AXIS2_PLACEMENT_3D ( 'NONE', #3182, #198, #6056 ) ;
#9683 = DIRECTION ( 'NONE',  ( 1.000000000000000000, -1.010728034814421376E-30, -1.090846720500930387E-30 ) ) ;
#9684 = CYLINDRICAL_SURFACE ( 'NONE', #9706, 4.000000000000008882 ) ;
#9685 = ORIENTED_EDGE ( 'NONE', *, *, #12400, .F. ) ;
#9686 = CARTESIAN_POINT ( 'NONE',  ( 28.99999999999999645, 3.469446951953614189E-15, 0.000000000000000000 ) ) ;
#9687 = DIRECTION ( 'NONE',  ( -1.848892746611742259E-31, 1.000000000000000000, -3.250006781153460502E-32 ) ) ;
#9688 = EDGE_CURVE ( 'NONE', #9180, #4888, #8013, .T. ) ;
#9689 = EDGE_CURVE ( 'NONE', #3082, #4835, #6505, .T. ) ;
#9690 = VERTEX_POINT ( 'NONE', #12241 ) ;
#9691 = ORIENTED_EDGE ( 'NONE', *, *, #10680, .T. ) ;
#9692 = ORIENTED_EDGE ( 'NONE', *, *, #7001, .T. ) ;
#9693 = LINE ( 'NONE', #888, #4170 ) ;
#9694 = VERTEX_POINT ( 'NONE', #8428 ) ;
#9695 = CARTESIAN_POINT ( 'NONE',  ( 0.000000000000000000, 0.000000000000000000, 0.000000000000000000 ) ) ;
#9696 = EDGE_LOOP ( 'NONE', ( #2856, #790 ) ) ;
#9697 = DIRECTION ( 'NONE',  ( -1.000000000000000000, 1.010728034814421376E-30, 1.090846720500930387E-30 ) ) ;
#9698 = AXIS2_PLACEMENT_3D ( 'NONE', #11941, #11029, #272 ) ;
#9699 = CIRCLE ( 'NONE', #3372, 6.499000000000009436 ) ;
#9700 = DIRECTION ( 'NONE',  ( 0.000000000000000000, -5.551115123125775923E-17, -1.000000000000000000 ) ) ;
#9701 = ADVANCED_BREP_SHAPE_REPRESENTATION ( '', ( #10029, #12422 ), #5765 ) ;
#9702 = EDGE_CURVE ( 'NONE', #11575, #5257, #9647, .T. ) ;
#9703 = CARTESIAN_POINT ( 'NONE',  ( -35.00000000000006395, -2.157041537713704155E-29, 2.000000000000002220 ) ) ;
#9704 = ORIENTED_EDGE ( 'NONE', *, *, #5663, .F. ) ;
#9705 = CARTESIAN_POINT ( 'NONE',  ( 27.00000000000001421, 81.84122341717352356, -27.68198508464163510 ) ) ;
#9706 = AXIS2_PLACEMENT_3D ( 'NONE', #10852, #2902, #11774 ) ;
#9707 = ORIENTED_EDGE ( 'NONE', *, *, #7362, .F. ) ;
#9708 = AXIS2_PLACEMENT_3D ( 'NONE', #3816, #12645, #3936 ) ;
#9709 = DIRECTION ( 'NONE',  ( -1.000000000000000000, -5.916456789157576279E-31, 1.224646799147353947E-16 ) ) ;
#9710 = CIRCLE ( 'NONE', #265, 6.000000000000013323 ) ;
#9711 =( NAMED_UNIT ( * ) PLANE_ANGLE_UNIT ( ) SI_UNIT ( $, .RADIAN. ) );
#9712 = CARTESIAN_POINT ( 'NONE',  ( 19.99999999999999645, -5.682309657208357123, 3.313524683561968942 ) ) ;
#9713 = DIRECTION ( 'NONE',  ( -0.000000000000000000, -1.530455820933490821E-32, 1.000000000000000000 ) ) ;
#9714 = CIRCLE ( 'NONE', #2975, 2.800000000000003819 ) ;
#9715 = CARTESIAN_POINT ( 'NONE',  ( 0.000000000000000000, -6.969736844459680114, -2.486517307195217796 ) ) ;
#9716 = CARTESIAN_POINT ( 'NONE',  ( 40.00000000000000711, 21.47552320888931021, -7.222675303056226070 ) ) ;
#9717 = DIRECTION ( 'NONE',  ( -1.000000000000000000, 1.010728034814421376E-30, 1.090846720500930387E-30 ) ) ;
#9718 = EDGE_CURVE ( 'NONE', #6031, #11780, #10062, .T. ) ;
#9719 = CARTESIAN_POINT ( 'NONE',  ( 19.99999999999999645, -6.133480037816503305, 2.376659734729468010 ) ) ;
#9720 = EDGE_CURVE ( 'NONE', #10576, #11388, #4534, .T. ) ;
#9721 = DIRECTION ( 'NONE',  ( -1.000000000000000000, 1.010728034814421376E-30, 1.090846720500930387E-30 ) ) ;
#9722 = EDGE_CURVE ( 'NONE', #2041, #11058, #204, .T. ) ;
#9723 = DIRECTION ( 'NONE',  ( -1.000000000000000000, 1.010728034814421376E-30, 1.090846720500930387E-30 ) ) ;
#9724 = VECTOR ( 'NONE', #10343, 1000.000000000000000 ) ;
#9725 = ADVANCED_FACE ( 'NONE', ( #2580 ), #10416, .T. ) ;
#9726 = ORIENTED_EDGE ( 'NONE', *, *, #10571, .F. ) ;
#9727 = EDGE_LOOP ( 'NONE', ( #12722, #1694, #6494, #8446 ) ) ;
#9728 = CARTESIAN_POINT ( 'NONE',  ( 0.000000000000000000, 30.00000000000000000, 0.000000000000000000 ) ) ;
#9729 = CARTESIAN_POINT ( 'NONE',  ( 0.000000000000000000, -0.8865213383406727043, 1.535500000000009191 ) ) ;
#9730 = CARTESIAN_POINT ( 'NONE',  ( 2.000000000000001776, 0.000000000000000000, 1.535500000000000087 ) ) ;
#9731 = DIRECTION ( 'NONE',  ( -1.000000000000000000, 1.010728034814421376E-30, 1.090846720500930387E-30 ) ) ;
#9732 = VERTEX_POINT ( 'NONE', #12306 ) ;
#9733 = AXIS2_PLACEMENT_3D ( 'NONE', #11492, #6536, #5680 ) ;
#9734 = CARTESIAN_POINT ( 'NONE',  ( -31.74999999999995026, 0.000000000000000000, 6.938893903907228378E-15 ) ) ;
#9735 = AXIS2_PLACEMENT_3D ( 'NONE', #2840, #6878, #12554 ) ;
#9736 = DIRECTION ( 'NONE',  ( 0.000000000000000000, 0.000000000000000000, -1.000000000000000000 ) ) ;
#9737 = PRODUCT_DEFINITION_SHAPE ( 'NONE', 'NONE',  #12755 ) ;
#9738 = DIRECTION ( 'NONE',  ( -0.7071067811865504593, 0.000000000000000000, -0.7071067811865445751 ) ) ;
#9739 = ORIENTED_EDGE ( 'NONE', *, *, #333, .T. ) ;
#9740 = EDGE_LOOP ( 'NONE', ( #8285, #2952, #618, #7201 ) ) ;
#9741 = DIRECTION ( 'NONE',  ( 0.000000000000000000, 0.000000000000000000, 1.000000000000000000 ) ) ;
#9742 = EDGE_LOOP ( 'NONE', ( #4016, #8336 ) ) ;
#9743 = CIRCLE ( 'NONE', #4238, 2.200000000000003730 ) ;
#9744 = ORIENTED_EDGE ( 'NONE', *, *, #736, .T. ) ;
#9745 = VECTOR ( 'NONE', #1402, 1000.000000000000000 ) ;
#9746 = CARTESIAN_POINT ( 'NONE',  ( -1.654252653721905331, -3.663718938583013340, -0.01223254789873431253 ) ) ;
#9747 = ORIENTED_EDGE ( 'NONE', *, *, #3515, .T. ) ;
#9748 = DIRECTION ( 'NONE',  ( 0.000000000000000000, 1.530455820933490821E-32, -1.000000000000000000 ) ) ;
#9749 = DIRECTION ( 'NONE',  ( -0.000000000000000000, -1.000000000000000000, -0.000000000000000000 ) ) ;
#9750 = ORIENTED_EDGE ( 'NONE', *, *, #1500, .F. ) ;
#9751 = DIRECTION ( 'NONE',  ( 0.000000000000000000, 0.000000000000000000, 1.000000000000000000 ) ) ;
#9752 = UNCERTAINTY_MEASURE_WITH_UNIT (LENGTH_MEASURE( 1.000000000000000082E-05 ), #5584, 'distance_accuracy_value', 'NONE');
#9753 = CARTESIAN_POINT ( 'NONE',  ( 40.00000000000006395, 2.500000000000000000, -20.00000000000000000 ) ) ;
#9754 = CIRCLE ( 'NONE', #4216, 4.000000000000000000 ) ;
#9755 = VECTOR ( 'NONE', #1258, 1000.000000000000000 ) ;
#9756 = EDGE_LOOP ( 'NONE', ( #10729, #5393, #2023, #862 ) ) ;
#9757 = ORIENTED_EDGE ( 'NONE', *, *, #8694, .T. ) ;
#9758 = ORIENTED_EDGE ( 'NONE', *, *, #12484, .F. ) ;
#9759 = DIRECTION ( 'NONE',  ( -1.000000000000000000, 0.000000000000000000, 0.000000000000000000 ) ) ;
#9760 = VERTEX_POINT ( 'NONE', #1599 ) ;
#9761 = AXIS2_PLACEMENT_3D ( 'NONE', #12399, #7432, #10307 ) ;
#9762 = EDGE_CURVE ( 'NONE', #10785, #5894, #8838, .T. ) ;
#9763 = DIRECTION ( 'NONE',  ( 1.000000000000000000, -1.010728034814421376E-30, -1.090846720500930387E-30 ) ) ;
#9764 = ORIENTED_EDGE ( 'NONE', *, *, #6766, .F. ) ;
#9765 = DIRECTION ( 'NONE',  ( -1.577021341797098546E-16, -1.177425296209237084E-30, -1.000000000000000000 ) ) ;
#9766 = DIRECTION ( 'NONE',  ( -1.000000000000000000, 1.010728034814421376E-30, 1.090846720500930387E-30 ) ) ;
#9767 = AXIS2_PLACEMENT_3D ( 'NONE', #11152, #3251, #6127 ) ;
#9768 = FACE_OUTER_BOUND ( 'NONE', #11708, .T. ) ;
#9769 = CIRCLE ( 'NONE', #5480, 2.149999999999999023 ) ;
#9770 = VERTEX_POINT ( 'NONE', #12434 ) ;
#9771 = DIRECTION ( 'NONE',  ( -0.7071067811865348052, 4.734329415644857690E-17, -0.7071067811865602293 ) ) ;
#9772 = ORIENTED_EDGE ( 'NONE', *, *, #9231, .F. ) ;
#9773 = FACE_OUTER_BOUND ( 'NONE', #1419, .T. ) ;
#9774 = FILL_AREA_STYLE_COLOUR ( '', #12577 ) ;
#9775 = EDGE_CURVE ( 'NONE', #7469, #6684, #1471, .T. ) ;
#9776 = CYLINDRICAL_SURFACE ( 'NONE', #1231, 2.800000000000003819 ) ;
#9777 = ADVANCED_FACE ( 'NONE', ( #11464, #2648, #2635, #2500 ), #3408, .T. ) ;
#9778 = EDGE_CURVE ( 'NONE', #9551, #2818, #9297, .T. ) ;
#9779 = CIRCLE ( 'NONE', #6514, 2.800000000000003819 ) ;
#9780 = DIRECTION ( 'NONE',  ( -1.000000000000000000, 1.332267629550187849E-14, 0.000000000000000000 ) ) ;
#9781 = AXIS2_PLACEMENT_3D ( 'NONE', #4013, #7933, #6199 ) ;
#9782 = CARTESIAN_POINT ( 'NONE',  ( 19.99999999999997868, -7.301715115245761112, -1.202063382601588959 ) ) ;
#9783 = CARTESIAN_POINT ( 'NONE',  ( 3.122502256758252770E-14, -4.618802153517026277, -3.504271511727134580 ) ) ;
#9784 = CARTESIAN_POINT ( 'NONE',  ( 4.197393957002303999, 7.389034437926038210E-14, -3.503767560748934251 ) ) ;
#9785 = CARTESIAN_POINT ( 'NONE',  ( 19.99999999999999645, 0.000000000000000000, 0.000000000000000000 ) ) ;
#9786 = CARTESIAN_POINT ( 'NONE',  ( 40.00000000000000711, 18.52447679111068268, -16.77732469694377926 ) ) ;
#9787 = CIRCLE ( 'NONE', #8774, 2.149999999999999023 ) ;
#9788 = LINE ( 'NONE', #11810, #6836 ) ;
#9789 = VERTEX_POINT ( 'NONE', #4555 ) ;
#9790 = ORIENTED_EDGE ( 'NONE', *, *, #2758, .T. ) ;
#9791 = CYLINDRICAL_SURFACE ( 'NONE', #690, 3.500000000000000000 ) ;
#9792 = CARTESIAN_POINT ( 'NONE',  ( 4.000000000000000000, -1.942223658245634255, -0.3516579909967644801 ) ) ;
#9793 = DIRECTION ( 'NONE',  ( 1.000000000000000000, 1.849040895279789448E-31, -6.938893903907224680E-17 ) ) ;
#9794 = DIRECTION ( 'NONE',  ( 2.218671295934093250E-30, -5.551115123125776539E-17, -1.000000000000000000 ) ) ;
#9795 = EDGE_LOOP ( 'NONE', ( #55, #546, #9026, #4213 ) ) ;
#9796 = DIRECTION ( 'NONE',  ( 0.000000000000000000, -1.530455820933490821E-32, 1.000000000000000000 ) ) ;
#9797 = FACE_OUTER_BOUND ( 'NONE', #11124, .T. ) ;
#9798 = ADVANCED_FACE ( 'NONE', ( #8346 ), #1389, .T. ) ;
#9799 = CYLINDRICAL_SURFACE ( 'NONE', #10073, 7.400000000000010125 ) ;
#9800 = ORIENTED_EDGE ( 'NONE', *, *, #6369, .T. ) ;
#9801 = VERTEX_POINT ( 'NONE', #8407 ) ;
#9802 = CYLINDRICAL_SURFACE ( 'NONE', #7820, 10.00000000000000178 ) ;
#9803 = ORIENTED_EDGE ( 'NONE', *, *, #3587, .F. ) ;
#9804 = ORIENTED_EDGE ( 'NONE', *, *, #5623, .T. ) ;
#9805 = PRODUCT_CONTEXT ( 'NONE', #5024, 'mechanical' ) ;
#9806 = VECTOR ( 'NONE', #9312, 1000.000000000000000 ) ;
#9807 = DIRECTION ( 'NONE',  ( -1.000000000000000000, 1.010728034814421376E-30, 1.090846720500930387E-30 ) ) ;
#9808 = VERTEX_POINT ( 'NONE', #7327 ) ;
#9809 = EDGE_CURVE ( 'NONE', #10658, #6823, #6422, .T. ) ;
#9810 = CARTESIAN_POINT ( 'NONE',  ( -5.384454397937084025, -2.799244553968360123E-15, -5.000000000000011546 ) ) ;
#9811 = EDGE_CURVE ( 'NONE', #10621, #11575, #11944, .T. ) ;
#9812 = CARTESIAN_POINT ( 'NONE',  ( 19.99999999999999645, -5.362766118793823367, -3.671204237728701969 ) ) ;
#9813 = ORIENTED_EDGE ( 'NONE', *, *, #5924, .T. ) ;
#9814 = CARTESIAN_POINT ( 'NONE',  ( -10.00000000000000178, 0.000000000000000000, 0.000000000000000000 ) ) ;
#9815 = CYLINDRICAL_SURFACE ( 'NONE', #4422, 6.499000000000010324 ) ;
#9816 = ORIENTED_EDGE ( 'NONE', *, *, #6646, .T. ) ;
#9817 = ORIENTED_EDGE ( 'NONE', *, *, #6469, .T. ) ;
#9818 = ORIENTED_EDGE ( 'NONE', *, *, #658, .F. ) ;
#9819 = DIRECTION ( 'NONE',  ( 0.000000000000000000, 0.000000000000000000, -1.000000000000000000 ) ) ;
#9820 = ORIENTED_EDGE ( 'NONE', *, *, #6816, .T. ) ;
#9821 = CARTESIAN_POINT ( 'NONE',  ( 0.000000000000000000, -6.182645281642484392, -2.245659411033197550 ) ) ;
#9822 = VECTOR ( 'NONE', #10643, 1000.000000000000000 ) ;
#9823 = ORIENTED_EDGE ( 'NONE', *, *, #7963, .T. ) ;
#9824 = EDGE_CURVE ( 'NONE', #9407, #1153, #7216, .T. ) ;
#9825 = EDGE_CURVE ( 'NONE', #9222, #8136, #11732, .T. ) ;
#9826 = CARTESIAN_POINT ( 'NONE',  ( -0.02448733951237958006, -4.877042772274735150, -3.751161874094032012 ) ) ;
#9827 = AXIS2_PLACEMENT_3D ( 'NONE', #8040, #10743, #961 ) ;
#9828 = VECTOR ( 'NONE', #9763, 1000.000000000000000 ) ;
#9829 = CARTESIAN_POINT ( 'NONE',  ( 9.999999999999998224, 3.975087478966743415, -6.241688836730176604 ) ) ;
#9830 = EDGE_CURVE ( 'NONE', #12174, #8613, #361, .T. ) ;
#9831 = ORIENTED_EDGE ( 'NONE', *, *, #448, .T. ) ;
#9832 = AXIS2_PLACEMENT_3D ( 'NONE', #9619, #12617, #1721 ) ;
#9833 = DIRECTION ( 'NONE',  ( 0.000000000000000000, 0.000000000000000000, 1.000000000000000000 ) ) ;
#9834 = ORIENTED_EDGE ( 'NONE', *, *, #6011, .T. ) ;
#9835 = DIRECTION ( 'NONE',  ( 0.000000000000000000, 0.000000000000000000, 1.000000000000000000 ) ) ;
#9836 = DIRECTION ( 'NONE',  ( 1.848892746611746419E-31, 1.000000000000000000, -3.250006781153460502E-32 ) ) ;
#9837 = AXIS2_PLACEMENT_3D ( 'NONE', #9719, #4846, #10886 ) ;
#9838 = EDGE_CURVE ( 'NONE', #865, #11564, #3114, .T. ) ;
#9839 = DIRECTION ( 'NONE',  ( -1.140150527077241873E-30, 0.000000000000000000, 1.000000000000000000 ) ) ;
#9840 = PRODUCT_DEFINITION_SHAPE ( 'NONE', 'NONE',  #12758 ) ;
#9841 = CYLINDRICAL_SURFACE ( 'NONE', #968, 7.400000000000010125 ) ;
#9842 = VECTOR ( 'NONE', #10615, 1000.000000000000000 ) ;
#9843 = CARTESIAN_POINT ( 'NONE',  ( 27.00000000000001421, 81.84122341717352356, -2.681985084641642203 ) ) ;
#9844 = LINE ( 'NONE', #7746, #729 ) ;
#9845 = DIRECTION ( 'NONE',  ( -1.000000000000000000, 1.010728034814421376E-30, 1.090846720500930387E-30 ) ) ;
#9846 = ADVANCED_FACE ( 'NONE', ( #489, #4419 ), #2373, .F. ) ;
#9847 = FACE_OUTER_BOUND ( 'NONE', #2232, .T. ) ;
#9848 = ADVANCED_FACE ( 'NONE', ( #6288 ), #10261, .T. ) ;
#9849 = CIRCLE ( 'NONE', #2481, 6.499000000000009436 ) ;
#9850 = AXIS2_PLACEMENT_3D ( 'NONE', #6085, #8916, #100 ) ;
#9851 = CARTESIAN_POINT ( 'NONE',  ( 9.999999999999994671, 1.528443194675403349, 7.240432404259464327 ) ) ;
#9852 =( REPRESENTATION_RELATIONSHIP ('NONE','NONE', #10018, #71 ) REPRESENTATION_RELATIONSHIP_WITH_TRANSFORMATION ( #10314 )SHAPE_REPRESENTATION_RELATIONSHIP( ) );
#9853 = ORIENTED_EDGE ( 'NONE', *, *, #7773, .F. ) ;
#9854 = ORIENTED_EDGE ( 'NONE', *, *, #4181, .F. ) ;
#9855 = CARTESIAN_POINT ( 'NONE',  ( 20.00000000000006750, -4.500000000000000000, -20.00000000000000000 ) ) ;
#9856 = CIRCLE ( 'NONE', #6796, 6.499000000000008548 ) ;
#9857 = DIRECTION ( 'NONE',  ( 0.000000000000000000, 1.000000000000000000, -8.560894001270036306E-16 ) ) ;
#9858 = CARTESIAN_POINT ( 'NONE',  ( 33.00000000000001421, 39.34792583643766761, -17.06347054209568270 ) ) ;
#9859 = CIRCLE ( 'NONE', #7217, 1.535500000000000087 ) ;
#9860 = VECTOR ( 'NONE', #3181, 1000.000000000000114 ) ;
#9861 = CARTESIAN_POINT ( 'NONE',  ( 2.000000000000001776, 1.773042676681341856, -3.469446951953614189E-15 ) ) ;
#9862 = ORIENTED_EDGE ( 'NONE', *, *, #8439, .T. ) ;
#9863 = CARTESIAN_POINT ( 'NONE',  ( 33.00000000000000711, 58.55522666905708462, -36.77936687539386185 ) ) ;
#9864 = CARTESIAN_POINT ( 'NONE',  ( -5.560781378645556217, -3.469446951953614189E-15, -4.000000000000010658 ) ) ;
#9865 = FACE_OUTER_BOUND ( 'NONE', #3099, .T. ) ;
#9866 = EDGE_LOOP ( 'NONE', ( #8541, #10957, #4805, #2311 ) ) ;
#9867 = VERTEX_POINT ( 'NONE', #5383 ) ;
#9868 = DIRECTION ( 'NONE',  ( 0.000000000000000000, 0.000000000000000000, 1.000000000000000000 ) ) ;
#9869 = EDGE_LOOP ( 'NONE', ( #3858, #8440, #172, #4762 ) ) ;
#9870 = COLOUR_RGB ( '', 0.09019608, 0.27058824, 0.51372549) ;
#9871 = VERTEX_POINT ( 'NONE', #3472 ) ;
#9872 = APPLICATION_PROTOCOL_DEFINITION ( 'draft international standard', 'automotive_design', 1998, #7485 ) ;
#9873 = DIRECTION ( 'NONE',  ( 0.000000000000000000, 0.000000000000000000, 1.000000000000000000 ) ) ;
#9874 = VERTEX_POINT ( 'NONE', #7386 ) ;
#9875 = DIRECTION ( 'NONE',  ( 0.000000000000000000, 0.3513748240813434620, -0.9362348706397368714 ) ) ;
#9876 = EDGE_CURVE ( 'NONE', #6211, #11663, #5149, .T. ) ;
#9877 = DIRECTION ( 'NONE',  ( 0.000000000000000000, 0.000000000000000000, 1.000000000000000000 ) ) ;
#9878 = ORIENTED_EDGE ( 'NONE', *, *, #4335, .T. ) ;
#9879 = DIRECTION ( 'NONE',  ( 0.000000000000000000, -1.530455820933490821E-32, 1.000000000000000000 ) ) ;
#9880 = PLANE ( 'NONE',  #4836 ) ;
#9881 = EDGE_CURVE ( 'NONE', #5977, #10545, #9358, .T. ) ;
#9882 = ORIENTED_EDGE ( 'NONE', *, *, #10009, .F. ) ;
#9883 = ORIENTED_EDGE ( 'NONE', *, *, #4283, .F. ) ;
#9884 = ADVANCED_FACE ( 'NONE', ( #3529 ), #7449, .T. ) ;
#9885 = ORIENTED_EDGE ( 'NONE', *, *, #772, .F. ) ;
#9886 = EDGE_CURVE ( 'NONE', #711, #412, #10395, .T. ) ;
#9887 = DIRECTION ( 'NONE',  ( -1.000000000000000000, 1.010728034814421376E-30, 1.090846720500930387E-30 ) ) ;
#9888 = VECTOR ( 'NONE', #3456, 1000.000000000000000 ) ;
#9889 = CARTESIAN_POINT ( 'NONE',  ( 4.211405965630456549, 2.460463115436249293, -3.751298928144576106 ) ) ;
#9890 = ORIENTED_EDGE ( 'NONE', *, *, #7623, .T. ) ;
#9891 = EDGE_CURVE ( 'NONE', #5778, #2655, #621, .T. ) ;
#9892 = FACE_OUTER_BOUND ( 'NONE', #2797, .T. ) ;
#9893 = ORIENTED_EDGE ( 'NONE', *, *, #8630, .T. ) ;
#9894 = CARTESIAN_POINT ( 'NONE',  ( 19.99999999999999645, 0.000000000000000000, 0.000000000000000000 ) ) ;
#9895 = CARTESIAN_POINT ( 'NONE',  ( 4.236525694536561026, -2.416953475386480754, -3.751298745799842571 ) ) ;
#9896 = DIRECTION ( 'NONE',  ( -1.000000000000000000, 1.010728034814421376E-30, 1.090846720500930387E-30 ) ) ;
#9897 = EDGE_LOOP ( 'NONE', ( #5910, #4100, #8121, #5233, #2453 ) ) ;
#9898 = FACE_OUTER_BOUND ( 'NONE', #10465, .T. ) ;
#9899 = ORIENTED_EDGE ( 'NONE', *, *, #9531, .F. ) ;
#9900 = DIRECTION ( 'NONE',  ( -1.000000000000000000, 1.010728034814421376E-30, 1.090846720500930387E-30 ) ) ;
#9901 = CLOSED_SHELL ( 'NONE', ( #2678, #6123, #7109, #5420, #12038, #5098, #4266, #1129, #11354, #5725, #5260, #3583, #4660, #7053, #4824 ) ) ;
#9902 = DIRECTION ( 'NONE',  ( 1.140150527077241873E-30, 0.000000000000000000, -1.000000000000000000 ) ) ;
#9903 = VECTOR ( 'NONE', #2329, 1000.000000000000114 ) ;
#9904 = LINE ( 'NONE', #5097, #12594 ) ;
#9905 = CARTESIAN_POINT ( 'NONE',  ( 14.00000000000000000, 30.00000000000000000, -6.000000000000000000 ) ) ;
#9906 = CARTESIAN_POINT ( 'NONE',  ( 19.99999999999997868, 1.052479792859146723, -6.413211932068299426 ) ) ;
#9907 = CARTESIAN_POINT ( 'NONE',  ( 40.00000000000006395, 1.290960574571364216E-15, -20.00000000000000000 ) ) ;
#9908 = CARTESIAN_POINT ( 'NONE',  ( 9.757359312880696578, -13.00000000000000000, -4.242640687119267895 ) ) ;
#9909 = CIRCLE ( 'NONE', #2124, 2.500000000000000888 ) ;
#9910 = CIRCLE ( 'NONE', #7674, 1.535500000000001863 ) ;
#9911 = CARTESIAN_POINT ( 'NONE',  ( 2.000000000000001776, 1.773042676681341856, -3.469446951953614189E-15 ) ) ;
#9912 = CARTESIAN_POINT ( 'NONE',  ( 0.000000000000000000, 4.494880553659092115, -4.802513683199192585 ) ) ;
#9913 = EDGE_CURVE ( 'NONE', #9038, #11856, #9856, .T. ) ;
#9914 = VECTOR ( 'NONE', #2233, 1000.000000000000000 ) ;
#9915 = ORIENTED_EDGE ( 'NONE', *, *, #326, .F. ) ;
#9916 = DIRECTION ( 'NONE',  ( -1.000000000000000000, -1.031065855027150586E-29, -2.218671295934092550E-30 ) ) ;
#9917 = EDGE_CURVE ( 'NONE', #568, #9126, #7638, .T. ) ;
#9918 = CARTESIAN_POINT ( 'NONE',  ( 40.00000000000006395, 4.500000000000000000, -20.00000000000000000 ) ) ;
#9919 = MANIFOLD_SOLID_BREP ( 'Move Face1', #2746 ) ;
#9920 = CARTESIAN_POINT ( 'NONE',  ( 9.999999999999998224, 7.380072687735817816, 0.5427035320837020338 ) ) ;
#9921 = LINE ( 'NONE', #2013, #4289 ) ;
#9922 = DIRECTION ( 'NONE',  ( 1.000000000000000000, 0.000000000000000000, 0.000000000000000000 ) ) ;
#9923 = ORIENTED_EDGE ( 'NONE', *, *, #12486, .T. ) ;
#9924 = DIRECTION ( 'NONE',  ( -1.000000000000000000, 1.010728034814421376E-30, 1.090846720500930387E-30 ) ) ;
#9925 = PLANE ( 'NONE',  #4621 ) ;
#9926 = FACE_OUTER_BOUND ( 'NONE', #2697, .T. ) ;
#9927 = ORIENTED_EDGE ( 'NONE', *, *, #9720, .T. ) ;
#9928 = VECTOR ( 'NONE', #6730, 1000.000000000000000 ) ;
#9929 = VERTEX_POINT ( 'NONE', #2765 ) ;
#9930 = DIRECTION ( 'NONE',  ( 1.000000000000000000, 0.000000000000000000, 0.000000000000000000 ) ) ;
#9931 = ORIENTED_EDGE ( 'NONE', *, *, #11450, .T. ) ;
#9932 = ORIENTED_EDGE ( 'NONE', *, *, #10803, .T. ) ;
#9933 = SHAPE_DEFINITION_REPRESENTATION ( #11104, #4436 ) ;
#9934 = DIRECTION ( 'NONE',  ( 1.000000000000000000, 0.000000000000000000, 0.000000000000000000 ) ) ;
#9935 = ORIENTED_EDGE ( 'NONE', *, *, #695, .F. ) ;
#9936 = CYLINDRICAL_SURFACE ( 'NONE', #8406, 6.499000000000010324 ) ;
#9937 = CARTESIAN_POINT ( 'NONE',  ( 19.99999999999999645, 0.000000000000000000, 0.000000000000000000 ) ) ;
#9938 = ADVANCED_FACE ( 'NONE', ( #741 ), #1646, .T. ) ;
#9939 = VERTEX_POINT ( 'NONE', #8665 ) ;
#9940 = CIRCLE ( 'NONE', #2784, 2.800000000000003375 ) ;
#9941 = CARTESIAN_POINT ( 'NONE',  ( 40.00000000000000711, 15.24625277455639250, -6.248133273622505257 ) ) ;
#9942 = DIRECTION ( 'NONE',  ( -1.000000000000000000, 1.010728034814421376E-30, 1.090846720500930387E-30 ) ) ;
#9943 = VERTEX_POINT ( 'NONE', #864 ) ;
#9944 = AXIS2_PLACEMENT_3D ( 'NONE', #9282, #5302, #407 ) ;
#9945 = ORIENTED_EDGE ( 'NONE', *, *, #6174, .F. ) ;
#9946 = ORIENTED_EDGE ( 'NONE', *, *, #11215, .T. ) ;
#9947 = ORIENTED_EDGE ( 'NONE', *, *, #9957, .F. ) ;
#9948 = DIRECTION ( 'NONE',  ( 1.000000000000000000, -1.010728034814421376E-30, -1.090846720500930387E-30 ) ) ;
#9949 = VERTEX_POINT ( 'NONE', #6679 ) ;
#9950 = ADVANCED_FACE ( 'NONE', ( #3775 ), #4802, .T. ) ;
#9951 = FACE_OUTER_BOUND ( 'NONE', #9316, .T. ) ;
#9952 = ORIENTED_EDGE ( 'NONE', *, *, #1847, .F. ) ;
#9953 = AXIS2_PLACEMENT_3D ( 'NONE', #4244, #9000, #9130 ) ;
#9954 = EDGE_CURVE ( 'NONE', #12437, #9038, #6805, .T. ) ;
#9955 = AXIS2_PLACEMENT_3D ( 'NONE', #8986, #1007, #3855 ) ;
#9956 = CARTESIAN_POINT ( 'NONE',  ( 19.99999999999997868, 6.557268578288196537, 0.5199208220222073518 ) ) ;
#9957 = EDGE_CURVE ( 'NONE', #12437, #10909, #9252, .T. ) ;
#9958 = DIRECTION ( 'NONE',  ( 0.000000000000000000, 0.2660368455666687892, 0.9639628606958550172 ) ) ;
#9959 = DIRECTION ( 'NONE',  ( 0.000000000000000000, 0.8345732537212999791, 0.5508969814521064157 ) ) ;
#9960 = EDGE_CURVE ( 'NONE', #11636, #11649, #11742, .T. ) ;
#9961 = ORIENTED_EDGE ( 'NONE', *, *, #4360, .T. ) ;
#9962 = DIRECTION ( 'NONE',  ( 0.000000000000000000, 0.000000000000000000, 1.000000000000000000 ) ) ;
#9963 = AXIS2_PLACEMENT_3D ( 'NONE', #2645, #4372, #8297 ) ;
#9964 = ORIENTED_EDGE ( 'NONE', *, *, #8953, .F. ) ;
#9965 = DIRECTION ( 'NONE',  ( 0.000000000000000000, 0.8660254037844380415, -0.5000000000000012212 ) ) ;
#9966 = CARTESIAN_POINT ( 'NONE',  ( 2.000000000000001776, 0.000000000000000000, 0.000000000000000000 ) ) ;
#9967 = ADVANCED_FACE ( 'NONE', ( #8533 ), #1773, .T. ) ;
#9968 = CARTESIAN_POINT ( 'NONE',  ( 15.00000000000003375, -12.49999999999999645, 3.994800001834461867E-31 ) ) ;
#9969 = ADVANCED_FACE ( 'NONE', ( #801 ), #633, .T. ) ;
#9970 = DIRECTION ( 'NONE',  ( -1.000000000000000000, 1.010728034814421376E-30, 1.090846720500930387E-30 ) ) ;
#9971 = CARTESIAN_POINT ( 'NONE',  ( 14.00000000000000000, 61.31370849898475228, 0.000000000000000000 ) ) ;
#9972 = CARTESIAN_POINT ( 'NONE',  ( 19.99999999999997868, 5.895746314278407674, -2.916892913127022702 ) ) ;
#9973 = DIRECTION ( 'NONE',  ( 0.000000000000000000, -0.2951046417778627751, -0.9554649393887560960 ) ) ;
#9974 = B_SPLINE_CURVE_WITH_KNOTS ( 'NONE', 3,
 ( #7523, #11460, #2641, #12301, #6561, #10477 ),
 .UNSPECIFIED., .F., .F.,
 ( 4, 2, 4 ),
 ( 0.002365888236227965159, 0.003551327329835074573, 0.004736766423442183988 ),
 .UNSPECIFIED. ) ;
#9975 = DIRECTION ( 'NONE',  ( 1.000000000000000000, -0.000000000000000000, -0.000000000000000000 ) ) ;
#9976 = PRESENTATION_LAYER_ASSIGNMENT (  '', '', ( #4240 ) ) ;
#9977 = ORIENTED_EDGE ( 'NONE', *, *, #7584, .F. ) ;
#9978 = DIRECTION ( 'NONE',  ( -1.000000000000000000, -5.916456789157575403E-31, 1.577021341797098793E-16 ) ) ;
#9979 = PLANE ( 'NONE',  #3981 ) ;
#9980 = DIRECTION ( 'NONE',  ( -1.000000000000000000, -5.916456789157575403E-31, 1.577021341797098793E-16 ) ) ;
#9981 = CARTESIAN_POINT ( 'NONE',  ( 19.99999999999999645, 0.000000000000000000, 0.000000000000000000 ) ) ;
#9982 = CARTESIAN_POINT ( 'NONE',  ( 19.99999999999999645, 0.000000000000000000, 0.000000000000000000 ) ) ;
#9983 = ORIENTED_EDGE ( 'NONE', *, *, #6786, .T. ) ;
#9984 = EDGE_CURVE ( 'NONE', #4020, #8922, #7569, .T. ) ;
#9985 = CARTESIAN_POINT ( 'NONE',  ( -30.00000000000000000, 19.99999999999999645, 2.000000000000001776 ) ) ;
#9986 = VECTOR ( 'NONE', #6005, 1000.000000000000000 ) ;
#9987 = CARTESIAN_POINT ( 'NONE',  ( 0.000000000000000000, 0.000000000000000000, 0.000000000000000000 ) ) ;
#9988 = VECTOR ( 'NONE', #3465, 1000.000000000000000 ) ;
#9989 = EDGE_CURVE ( 'NONE', #8740, #9308, #4863, .T. ) ;
#9990 = ORIENTED_EDGE ( 'NONE', *, *, #4552, .T. ) ;
#9991 = CARTESIAN_POINT ( 'NONE',  ( 19.99999999999999645, -1.966014849757073968, 6.277170897746257694 ) ) ;
#9992 = ORIENTED_EDGE ( 'NONE', *, *, #576, .F. ) ;
#9993 = ORIENTED_EDGE ( 'NONE', *, *, #7391, .F. ) ;
#9994 = CARTESIAN_POINT ( 'NONE',  ( 0.000000000000000000, 0.000000000000000000, 0.000000000000000000 ) ) ;
#9995 = AXIS2_PLACEMENT_3D ( 'NONE', #2585, #11534, #8621 ) ;
#9996 = CARTESIAN_POINT ( 'NONE',  ( 19.99999999999999645, -6.453973581750240385, 0.7636923504068631186 ) ) ;
#9997 = ORIENTED_EDGE ( 'NONE', *, *, #2189, .T. ) ;
#9998 = AXIS2_PLACEMENT_3D ( 'NONE', #7174, #9092, #11882 ) ;
#9999 = DIRECTION ( 'NONE',  ( -1.121661599611125110E-30, 0.9989930665413144784, 0.04486483035051876817 ) ) ;
#10000 = AXIS2_PLACEMENT_3D ( 'NONE', #12071, #3197, #3262 ) ;
#10001 = CARTESIAN_POINT ( 'NONE',  ( 2.000000000000001776, 0.000000000000000000, 0.000000000000000000 ) ) ;
#10002 = EDGE_LOOP ( 'NONE', ( #6034, #4966, #12212, #10764 ) ) ;
#10003 = CARTESIAN_POINT ( 'NONE',  ( 34.00000000000000000, 0.000000000000000000, -1.734723475976807094E-14 ) ) ;
#10004 = CARTESIAN_POINT ( 'NONE',  ( -11.83215956619923226, -30.00000000000000000, -2.000000000000000888 ) ) ;
#10005 = CARTESIAN_POINT ( 'NONE',  ( 0.000000000000000000, 0.000000000000000000, 0.000000000000000000 ) ) ;
#10006 = EDGE_LOOP ( 'NONE', ( #8934, #12530, #9818, #11367 ) ) ;
#10007 = ORIENTED_EDGE ( 'NONE', *, *, #6653, .T. ) ;
#10008 = VECTOR ( 'NONE', #11586, 1000.000000000000000 ) ;
#10009 = EDGE_CURVE ( 'NONE', #1458, #7604, #2157, .T. ) ;
#10010 = EDGE_LOOP ( 'NONE', ( #7726, #159, #7262, #6978 ) ) ;
#10011 = EDGE_CURVE ( 'NONE', #742, #6622, #8848, .T. ) ;
#10012 = ADVANCED_FACE ( 'NONE', ( #4927 ), #3959, .F. ) ;
#10013 = ORIENTED_EDGE ( 'NONE', *, *, #1285, .F. ) ;
#10014 = CARTESIAN_POINT ( 'NONE',  ( -35.00000000000006395, -19.99999999999999645, 2.000000000000006661 ) ) ;
#10015 = CARTESIAN_POINT ( 'NONE',  ( 4.000000000000001776, 1.658577278524726584, -3.531553309553335129 ) ) ;
#10016 = ORIENTED_EDGE ( 'NONE', *, *, #268, .F. ) ;
#10017 = CYLINDRICAL_SURFACE ( 'NONE', #3690, 7.400000000000010125 ) ;
#10018 = SHAPE_REPRESENTATION ( 'BR-598', ( #757, #7349, #965, #9995, #3658, #10830, #11871, #4668, #4259, #8369, #6110, #560, #6534, #6310, #10425, #4467, #11256 ), #10198 ) ;
#10019 = VERTEX_POINT ( 'NONE', #7942 ) ;
#10020 = LINE ( 'NONE', #8234, #3191 ) ;
#10021 = DIRECTION ( 'NONE',  ( 1.000000000000000000, -0.000000000000000000, -6.938893903907228378E-17 ) ) ;
#10022 = FACE_OUTER_BOUND ( 'NONE', #1668, .T. ) ;
#10023 = ORIENTED_EDGE ( 'NONE', *, *, #11447, .T. ) ;
#10024 = LINE ( 'NONE', #1217, #2033 ) ;
#10025 = ADVANCED_FACE ( 'NONE', ( #12013 ), #9799, .T. ) ;
#10026 = EDGE_LOOP ( 'NONE', ( #4746, #1146 ) ) ;
#10027 = CARTESIAN_POINT ( 'NONE',  ( -29.99999999999999289, 30.00000000000000000, 1.672083814130525448E-15 ) ) ;
#10028 = AXIS2_PLACEMENT_3D ( 'NONE', #9353, #2760, #6481 ) ;
#10029 = MANIFOLD_SOLID_BREP ( 'M4 Clearance Hole2', #12623 ) ;
#10030 = SURFACE_STYLE_USAGE ( .BOTH. , #1931 ) ;
#10031 = FACE_BOUND ( 'NONE', #7468, .T. ) ;
#10032 = DIRECTION ( 'NONE',  ( 0.000000000000000000, 0.000000000000000000, 1.000000000000000000 ) ) ;
#10033 = EDGE_CURVE ( 'NONE', #9099, #5519, #4544, .T. ) ;
#10034 = DIRECTION ( 'NONE',  ( 0.000000000000000000, 0.000000000000000000, 1.000000000000000000 ) ) ;
#10035 = DIRECTION ( 'NONE',  ( -1.000000000000000000, -1.031065855027150586E-29, 2.218671295934095703E-30 ) ) ;
#10036 = AXIS2_PLACEMENT_3D ( 'NONE', #1131, #10656, #11835 ) ;
#10037 = DIRECTION ( 'NONE',  ( 0.000000000000000000, 0.000000000000000000, 1.000000000000000000 ) ) ;
#10038 = CARTESIAN_POINT ( 'NONE',  ( 3.472371940586244321, 2.614027278893029660, -3.320322319201107764 ) ) ;
#10039 = EDGE_CURVE ( 'NONE', #5639, #802, #6183, .T. ) ;
#10040 = DIRECTION ( 'NONE',  ( 0.000000000000000000, 0.000000000000000000, 1.000000000000000000 ) ) ;
#10041 = EDGE_CURVE ( 'NONE', #2489, #11959, #3072, .T. ) ;
#10042 = AXIS2_PLACEMENT_3D ( 'NONE', #849, #137, #6851 ) ;
#10043 = AXIS2_PLACEMENT_3D ( 'NONE', #1921, #8752, #7786 ) ;
#10044 = CIRCLE ( 'NONE', #3301, 2.500000000000003553 ) ;
#10045 = ORIENTED_EDGE ( 'NONE', *, *, #695, .T. ) ;
#10046 = CARTESIAN_POINT ( 'NONE',  ( 20.00000000000000000, 22.56100271565320625, -6.249672610153678143 ) ) ;
#10047 = DIRECTION ( 'NONE',  ( -2.218671295934095002E-30, -5.551115123125776539E-17, -1.000000000000000000 ) ) ;
#10048 = CARTESIAN_POINT ( 'NONE',  ( -4.211399284164264678, 2.459729995988193973, -3.751162237960548929 ) ) ;
#10049 = CARTESIAN_POINT ( 'NONE',  ( 19.99999999999999645, 0.000000000000000000, 0.000000000000000000 ) ) ;
#10050 = ORIENTED_EDGE ( 'NONE', *, *, #11767, .T. ) ;
#10051 = DIRECTION ( 'NONE',  ( -1.224646799147352714E-16, -1.177425296209236909E-30, -1.000000000000000000 ) ) ;
#10052 = VECTOR ( 'NONE', #8631, 1000.000000000000000 ) ;
#10053 = AXIS2_PLACEMENT_3D ( 'NONE', #10557, #2594, #1613 ) ;
#10054 = CIRCLE ( 'NONE', #9232, 2.800000000000003375 ) ;
#10055 = CARTESIAN_POINT ( 'NONE',  ( 0.000000000000000000, 0.000000000000000000, 0.000000000000000000 ) ) ;
#10056 = PRODUCT_DEFINITION_SHAPE ( 'NONE', 'NONE',  #2740 ) ;
#10057 = CARTESIAN_POINT ( 'NONE',  ( 40.00000000000000000, 39.34792583643765340, -17.06347054209567560 ) ) ;
#10058 = ORIENTED_EDGE ( 'NONE', *, *, #6247, .F. ) ;
#10059 = FACE_OUTER_BOUND ( 'NONE', #5307, .T. ) ;
#10060 = ORIENTED_EDGE ( 'NONE', *, *, #11790, .F. ) ;
#10061 = ORIENTED_EDGE ( 'NONE', *, *, #12170, .F. ) ;
#10062 = CIRCLE ( 'NONE', #8024, 6.999999999999999112 ) ;
#10063 = DIRECTION ( 'NONE',  ( 0.000000000000000000, 5.551115123125777155E-17, 1.000000000000000000 ) ) ;
#10064 = AXIS2_PLACEMENT_3D ( 'NONE', #6016, #3076, #4214 ) ;
#10065 = ORIENTED_EDGE ( 'NONE', *, *, #1820, .F. ) ;
#10066 = ADVANCED_FACE ( 'NONE', ( #9865 ), #7116, .T. ) ;
#10067 = FACE_OUTER_BOUND ( 'NONE', #8979, .T. ) ;
#10068 = ORIENTED_EDGE ( 'NONE', *, *, #10964, .F. ) ;
#10069 = CARTESIAN_POINT ( 'NONE',  ( 20.00000000000000355, 14.86906044972263352, -7.469374795321336080 ) ) ;
#10070 = DIRECTION ( 'NONE',  ( -1.000000000000000000, 1.010728034814421376E-30, 1.090846720500930387E-30 ) ) ;
#10071 = DIRECTION ( 'NONE',  ( 0.000000000000000000, -0.4338837391175658365, 0.9009688679024154823 ) ) ;
#10072 = DIRECTION ( 'NONE',  ( -0.5000000000000056621, 5.798345671289627126E-17, -0.8660254037844352659 ) ) ;
#10073 = AXIS2_PLACEMENT_3D ( 'NONE', #2091, #6931, #4149 ) ;
#10074 = ORIENTED_EDGE ( 'NONE', *, *, #10996, .T. ) ;
#10075 = ORIENTED_EDGE ( 'NONE', *, *, #4542, .F. ) ;
#10076 = ORIENTED_EDGE ( 'NONE', *, *, #10919, .F. ) ;
#10077 = ORIENTED_EDGE ( 'NONE', *, *, #7927, .F. ) ;
#10078 = CARTESIAN_POINT ( 'NONE',  ( 19.99999999999999645, -3.730839900301562206, 5.321450426182494198 ) ) ;
#10079 = CARTESIAN_POINT ( 'NONE',  ( -15.00000000000000000, -19.99999999999998934, 12.00000000000002842 ) ) ;
#10080 = ORIENTED_EDGE ( 'NONE', *, *, #8614, .F. ) ;
#10081 = CARTESIAN_POINT ( 'NONE',  ( 4.000000000000000000, 0.9868501483902617499, -0.09357334158579612426 ) ) ;
#10082 =( GEOMETRIC_REPRESENTATION_CONTEXT ( 3 ) GLOBAL_UNCERTAINTY_ASSIGNED_CONTEXT ( ( #6504 ) ) GLOBAL_UNIT_ASSIGNED_CONTEXT ( ( #3934, #447, #11274 ) ) REPRESENTATION_CONTEXT ( 'NONE', 'WORKASPACE' ) );
#10083 = ORIENTED_EDGE ( 'NONE', *, *, #454, .T. ) ;
#10084 = DIRECTION ( 'NONE',  ( 0.000000000000000000, 0.000000000000000000, 1.000000000000000000 ) ) ;
#10085 = ADVANCED_FACE ( 'NONE', ( #4212 ), #8907, .T. ) ;
#10086 = ADVANCED_FACE ( 'NONE', ( #9926 ), #1118, .F. ) ;
#10087 = CARTESIAN_POINT ( 'NONE',  ( 0.000000000000000000, 0.000000000000000000, 0.000000000000000000 ) ) ;
#10088 = CARTESIAN_POINT ( 'NONE',  ( -45.00000000000012079, -19.99999999999999645, 3.443468848353431668E-15 ) ) ;
#10089 = ORIENTED_EDGE ( 'NONE', *, *, #6685, .T. ) ;
#10091 = CARTESIAN_POINT ( 'NONE',  ( 0.000000000000000000, 0.8865213383406622683, -1.535499999999995202 ) ) ;
#10090 = CIRCLE ( 'NONE', #11759, 2.800000000000003375 ) ;
#10092 = ORIENTED_EDGE ( 'NONE', *, *, #929, .T. ) ;
#10093 = CARTESIAN_POINT ( 'NONE',  ( 0.1999999999999987899, 0.000000000000000000, -1.734723475976807094E-14 ) ) ;
#10094 = SHAPE_REPRESENTATION ( 'socket head cap screw_iso_ISO 4762 M4 x 30 - 20N', ( #12422 ), #3119 ) ;
#10095 = CARTESIAN_POINT ( 'NONE',  ( -3.999999999999991562, 0.1981133338132476940, 6.974363408573500627E-15 ) ) ;
#10096 = AXIS2_PLACEMENT_3D ( 'NONE', #4581, #6574, #10291 ) ;
#10097 = DIRECTION ( 'NONE',  ( 1.000000000000000000, -0.000000000000000000, -6.938893903907228378E-17 ) ) ;
#10098 = VECTOR ( 'NONE', #9333, 1000.000000000000000 ) ;
#10099 = EDGE_CURVE ( 'NONE', #8975, #11564, #10970, .T. ) ;
#10100 = DIRECTION ( 'NONE',  ( 0.000000000000000000, 0.000000000000000000, 1.000000000000000000 ) ) ;
#10101 = APPLICATION_CONTEXT ( 'automotive_design' ) ;
#10102 = PLANE ( 'NONE',  #9767 ) ;
#10103 = PLANE ( 'NONE',  #12334 ) ;
#10104 = CARTESIAN_POINT ( 'NONE',  ( 2.836893136758657619, 3.208949435745621859, -3.505054077164843740 ) ) ;
#10105 = LINE ( 'NONE', #3499, #12597 ) ;
#10106 = AXIS2_PLACEMENT_3D ( 'NONE', #5159, #12056, #3245 ) ;
#10107 = SHAPE_REPRESENTATION_RELATIONSHIP ( 'NONE' , 'NONE' ,  #11514, #9701 ) ;
#10108 = VERTEX_POINT ( 'NONE', #5892 ) ;
#10109 = DIRECTION ( 'NONE',  ( -1.000000000000000000, 1.006188713385347367E-17, 3.844790828812615713E-17 ) ) ;
#10110 = CARTESIAN_POINT ( 'NONE',  ( 19.99999999999999645, -3.730839900301496925, -5.321450426182552818 ) ) ;
#10111 = CYLINDRICAL_SURFACE ( 'NONE', #4471, 2.800000000000003819 ) ;
#10112 = EDGE_CURVE ( 'NONE', #5079, #4568, #11824, .T. ) ;
#10113 = FACE_OUTER_BOUND ( 'NONE', #11986, .T. ) ;
#10114 = ORIENTED_EDGE ( 'NONE', *, *, #1422, .T. ) ;
#10115 = CIRCLE ( 'NONE', #10951, 2.800000000000004263 ) ;
#10116 = DIRECTION ( 'NONE',  ( -1.000000000000000000, -5.916456789157575403E-31, 1.224646799147352714E-16 ) ) ;
#10117 = AXIS2_PLACEMENT_3D ( 'NONE', #2181, #3415, #11192 ) ;
#10118 = EDGE_CURVE ( 'NONE', #10168, #2985, #3268, .T. ) ;
#10119 = DIRECTION ( 'NONE',  ( -6.938893903907224680E-17, 1.040834085586079721E-15, -1.000000000000000000 ) ) ;
#10120 = ORIENTED_EDGE ( 'NONE', *, *, #3773, .F. ) ;
#10121 = EDGE_CURVE ( 'NONE', #11062, #2497, #8329, .T. ) ;
#10122 = DIRECTION ( 'NONE',  ( 0.000000000000000000, 1.000000000000000000, 0.000000000000000000 ) ) ;
#10123 = ORIENTED_EDGE ( 'NONE', *, *, #1893, .F. ) ;
#10124 = CIRCLE ( 'NONE', #2767, 2.800000000000003819 ) ;
#10125 = ORIENTED_EDGE ( 'NONE', *, *, #1195, .T. ) ;
#10126 = ORIENTED_EDGE ( 'NONE', *, *, #5714, .T. ) ;
#10127 = SURFACE_STYLE_USAGE ( .BOTH. , #2425 ) ;
#10128 = DIRECTION ( 'NONE',  ( 0.000000000000000000, -0.8805955318567323387, -0.4738686624730092944 ) ) ;
#10129 = LINE ( 'NONE', #230, #9570 ) ;
#10130 = DIRECTION ( 'NONE',  ( 0.000000000000000000, -0.5877852522924801315, 0.8090169943749423442 ) ) ;
#10131 = CARTESIAN_POINT ( 'NONE',  ( 19.99999999999999645, -6.884685972239679153, 2.713134545806031195 ) ) ;
#10132 = PLANE ( 'NONE',  #2807 ) ;
#10133 = AXIS2_PLACEMENT_3D ( 'NONE', #2756, #5628, #1765 ) ;
#10134 = CARTESIAN_POINT ( 'NONE',  ( 0.000000000000000000, -0.8135880386783354012, 6.527339685683402060 ) ) ;
#10135 = EDGE_LOOP ( 'NONE', ( #2318, #491, #552, #2502 ) ) ;
#10136 = ORIENTED_EDGE ( 'NONE', *, *, #4840, .F. ) ;
#10137 = ORIENTED_EDGE ( 'NONE', *, *, #23, .T. ) ;
#10138 = ORIENTED_EDGE ( 'NONE', *, *, #9098, .T. ) ;
#10139 = CARTESIAN_POINT ( 'NONE',  ( 19.99999999999997868, 6.146182963951668299, 2.112211157443887100 ) ) ;
#10140 = CIRCLE ( 'NONE', #1925, 2.800000000000003819 ) ;
#10141 = CARTESIAN_POINT ( 'NONE',  ( -1.287237434361587551, -3.875615274277552036, -3.430618716626829379 ) ) ;
#10142 = ORIENTED_EDGE ( 'NONE', *, *, #11605, .T. ) ;
#10143 = CARTESIAN_POINT ( 'NONE',  ( 0.000000000000000000, -7.399010254356644722, -0.1210258481700102196 ) ) ;
#10144 = VERTEX_POINT ( 'NONE', #1501 ) ;
#10145 = CARTESIAN_POINT ( 'NONE',  ( -2.000000000000005329, 3.464101615137750390, 1.561251128379126385E-14 ) ) ;
#10146 = CARTESIAN_POINT ( 'NONE',  ( -1.747541505913285276, 3.837784562140254430, -3.503702292528920736 ) ) ;
#10147 = CYLINDRICAL_SURFACE ( 'NONE', #4834, 2.149999999999988809 ) ;
#10148 = DIRECTION ( 'NONE',  ( 1.000000000000000000, 1.031065855027150586E-29, -2.218671295934095703E-30 ) ) ;
#10149 = VERTEX_POINT ( 'NONE', #8391 ) ;
#10150 = ORIENTED_EDGE ( 'NONE', *, *, #2352, .T. ) ;
#10151 = LINE ( 'NONE', #7409, #6215 ) ;
#10152 = MANIFOLD_SOLID_BREP ( 'Bore', #4997 ) ;
#10153 = VECTOR ( 'NONE', #7215, 1000.000000000000227 ) ;
#10154 = DIRECTION ( 'NONE',  ( -1.000000000000000000, 0.000000000000000000, 0.000000000000000000 ) ) ;
#10155 = DIRECTION ( 'NONE',  ( -0.000000000000000000, -1.000000000000000000, -0.000000000000000000 ) ) ;
#10156 = CARTESIAN_POINT ( 'NONE',  ( 4.000000000000001776, -1.677850389431038591, -3.535268758347268836 ) ) ;
#10157 = DIRECTION ( 'NONE',  ( -0.000000000000000000, -1.000000000000000000, -0.000000000000000000 ) ) ;
#10158 = CIRCLE ( 'NONE', #6060, 6.000000000000013323 ) ;
#10159 = AXIS2_PLACEMENT_3D ( 'NONE', #5448, #6616, #11572 ) ;
#10160 = DIRECTION ( 'NONE',  ( -1.000000000000000000, 1.010728034814421376E-30, 1.090846720500930387E-30 ) ) ;
#10161 = ORIENTED_EDGE ( 'NONE', *, *, #5325, .T. ) ;
#10162 =( BOUNDED_SURFACE ( )  B_SPLINE_SURFACE ( 3, 2, ( 
 ( #8085, #359, #12031 ),
 ( #12163, #3282, #11183 ),
 ( #3222, #8280, #11120 ),
 ( #4288, #8217, #7134 ),
 ( #3342, #11057, #7263 ),
 ( #2372, #6285, #10193 ) ),
 .UNSPECIFIED., .F., .F., .T. ) 
 B_SPLINE_SURFACE_WITH_KNOTS ( ( 4, 2, 4 ),
 ( 3, 3 ),
 ( 0.02032853247518125531, 0.02278863295364820865, 0.02524873343211516200 ),
 ( 0.000000000000000000, 1.000000000000000000 ),
 .UNSPECIFIED. ) 
 GEOMETRIC_REPRESENTATION_ITEM ( )  RATIONAL_B_SPLINE_SURFACE ( (
 ( 1.000000000000000000, 0.8047781615896839602, 1.000000000000000000),
 ( 1.000000000000000000, 0.8123767586288903608, 1.000000000000000000),
 ( 1.000000000000000000, 0.8190662415564864407, 1.000000000000000000),
 ( 1.000000000000000000, 0.8192361015668554458, 1.000000000000000000),
 ( 1.000000000000000000, 0.8126135807104249986, 1.000000000000000000),
 ( 1.000000000000000000, 0.8047712338318581127, 1.000000000000000000) ) ) 
 REPRESENTATION_ITEM ( '' )  SURFACE ( )  );
#10163 = DIRECTION ( 'NONE',  ( 1.000000000000000000, -1.010728034814421376E-30, -1.090846720500930387E-30 ) ) ;
#10164 = DIRECTION ( 'NONE',  ( 0.000000000000000000, 0.4338837391175525693, 0.9009688679024219216 ) ) ;
#10165 = EDGE_CURVE ( 'NONE', #955, #8657, #11105, .T. ) ;
#10166 = EDGE_CURVE ( 'NONE', #2170, #10993, #540, .T. ) ;
#10167 = EDGE_CURVE ( 'NONE', #2096, #2020, #10044, .T. ) ;
#10168 = VERTEX_POINT ( 'NONE', #2291 ) ;
#10169 = AXIS2_PLACEMENT_3D ( 'NONE', #404, #8324, #1303 ) ;
#10170 = DIRECTION ( 'NONE',  ( 1.000000000000000000, -6.162975822039154730E-33, -4.563833282352349791E-17 ) ) ;
#10171 = FACE_OUTER_BOUND ( 'NONE', #7974, .T. ) ;
#10172 = MANIFOLD_SOLID_BREP ( 'Boss-Extrude2', #7664 ) ;
#10173 = CARTESIAN_POINT ( 'NONE',  ( -3.999999999999993339, -1.680117682357838316, -3.316611593219338072 ) ) ;
#10174 = CARTESIAN_POINT ( 'NONE',  ( 2.449848172108550326, 3.432307619358736961, -3.503702292528910522 ) ) ;
#10175 = LINE ( 'NONE', #5179, #11227 ) ;
#10176 = CARTESIAN_POINT ( 'NONE',  ( 3.469446951953614189E-14, -3.469446951953614189E-15, -4.484454397937126302 ) ) ;
#10177 = ORIENTED_EDGE ( 'NONE', *, *, #7627, .F. ) ;
#10178 = AXIS2_PLACEMENT_3D ( 'NONE', #8094, #10997, #1202 ) ;
#10179 = DIRECTION ( 'NONE',  ( -2.218671295934095002E-30, -5.551115123125776539E-17, -1.000000000000000000 ) ) ;
#10180 = VERTEX_POINT ( 'NONE', #472 ) ;
#10181 = EDGE_LOOP ( 'NONE', ( #12242, #6298, #10348, #5342 ) ) ;
#10182 = ITEM_DEFINED_TRANSFORMATION ( 'NONE', 'NONE', #560,  #12422 ) ;
#10183 = EDGE_LOOP ( 'NONE', ( #761, #11257, #8258, #1249 ) ) ;
#10184 = CARTESIAN_POINT ( 'NONE',  ( -0.3198814748697738075, -4.434118497892174382, -0.3507732604232444706 ) ) ;
#10185 = DIRECTION ( 'NONE',  ( 1.000000000000000000, 0.000000000000000000, 0.000000000000000000 ) ) ;
#10186 = CYLINDRICAL_SURFACE ( 'NONE', #4876, 10.00000000000002309 ) ;
#10187 = CARTESIAN_POINT ( 'NONE',  ( 14.00000000000000000, 30.00000000000000000, 0.000000000000000000 ) ) ;
#10188 = VECTOR ( 'NONE', #12726, 1000.000000000000000 ) ;
#10189 = DIRECTION ( 'NONE',  ( -1.000000000000000000, 0.000000000000000000, 1.159061634649218351E-16 ) ) ;
#10190 = ORIENTED_EDGE ( 'NONE', *, *, #9493, .F. ) ;
#10191 = ADVANCED_FACE ( 'NONE', ( #2420 ), #5366, .T. ) ;
#10192 = CIRCLE ( 'NONE', #12490, 2.800000000000002931 ) ;
#10193 = CARTESIAN_POINT ( 'NONE',  ( -4.236525694536565467, 2.416953475386456329, -3.751298745799851897 ) ) ;
#10194 = DIRECTION ( 'NONE',  ( -1.000000000000000000, 1.010728034814421376E-30, 1.090846720500930387E-30 ) ) ;
#10195 = VERTEX_POINT ( 'NONE', #2485 ) ;
#10196 = VERTEX_POINT ( 'NONE', #6401 ) ;
#10197 = ORIENTED_EDGE ( 'NONE', *, *, #6345, .T. ) ;
#10198 =( GEOMETRIC_REPRESENTATION_CONTEXT ( 3 ) GLOBAL_UNCERTAINTY_ASSIGNED_CONTEXT ( ( #9752 ) ) GLOBAL_UNIT_ASSIGNED_CONTEXT ( ( #5584, #10748, #4934 ) ) REPRESENTATION_CONTEXT ( 'NONE', 'WORKASPACE' ) );
#10199 = EDGE_LOOP ( 'NONE', ( #9878, #5246, #2978, #1474 ) ) ;
#10200 = VECTOR ( 'NONE', #5177, 1000.000000000000000 ) ;
#10201 = EDGE_CURVE ( 'NONE', #6567, #9308, #2042, .T. ) ;
#10202 = FACE_OUTER_BOUND ( 'NONE', #1698, .T. ) ;
#10203 = VECTOR ( 'NONE', #2805, 1000.000000000000000 ) ;
#10204 = ADVANCED_FACE ( 'NONE', ( #4539 ), #7556, .T. ) ;
#10205 = ORIENTED_EDGE ( 'NONE', *, *, #6320, .F. ) ;
#10206 = CARTESIAN_POINT ( 'NONE',  ( 3.999999999999999112, 1.941961291383485610, -0.3515519931180244861 ) ) ;
#10207 = VERTEX_POINT ( 'NONE', #1627 ) ;
#10208 = CARTESIAN_POINT ( 'NONE',  ( -4.211140560182161430, -2.431303136016561783, -3.745885042887451277 ) ) ;
#10209 = CYLINDRICAL_SURFACE ( 'NONE', #10782, 2.149999999999999023 ) ;
#10210 = CIRCLE ( 'NONE', #6093, 6.499000000000008548 ) ;
#10211 = LINE ( 'NONE', #7939, #1546 ) ;
#10212 = LINE ( 'NONE', #3241, #3500 ) ;
#10213 = ORIENTED_EDGE ( 'NONE', *, *, #9960, .F. ) ;
#10214 = ORIENTED_EDGE ( 'NONE', *, *, #9075, .F. ) ;
#10215 = DIRECTION ( 'NONE',  ( 0.000000000000000000, 0.000000000000000000, 1.000000000000000000 ) ) ;
#10216 = PRESENTATION_STYLE_ASSIGNMENT (( #7226 ) ) ;
#10217 = CARTESIAN_POINT ( 'NONE',  ( 20.00000000000000000, 16.67945018363952059, -6.690790236289298143 ) ) ;
#10218 = CARTESIAN_POINT ( 'NONE',  ( 6.000000000000000000, 49.63999999999998636, -13.00000000000000178 ) ) ;
#10219 = EDGE_CURVE ( 'NONE', #1526, #7722, #3701, .T. ) ;
#10220 = CARTESIAN_POINT ( 'NONE',  ( 19.99999999999999645, -4.046291478462229030, 5.186098161460289901 ) ) ;
#10221 = FACE_OUTER_BOUND ( 'NONE', #12599, .T. ) ;
#10222 = DIRECTION ( 'NONE',  ( -1.000000000000000000, 1.010728034814421376E-30, 1.090846720500930387E-30 ) ) ;
#10223 = ORIENTED_EDGE ( 'NONE', *, *, #8503, .T. ) ;
#10224 = DIRECTION ( 'NONE',  ( 0.000000000000000000, 0.000000000000000000, -1.000000000000000000 ) ) ;
#10225 = DIRECTION ( 'NONE',  ( 0.000000000000000000, 0.1785568947986370392, -0.9839295885986295565 ) ) ;
#10226 = EDGE_CURVE ( 'NONE', #9151, #9558, #8515, .T. ) ;
#10227 = ORIENTED_EDGE ( 'NONE', *, *, #3496, .T. ) ;
#10228 = DIRECTION ( 'NONE',  ( 1.140150527077241873E-30, 0.000000000000000000, -1.000000000000000000 ) ) ;
#10229 = DIRECTION ( 'NONE',  ( -1.000000000000000000, 1.010728034814421376E-30, 1.090846720500930387E-30 ) ) ;
#10230 = AXIS2_PLACEMENT_3D ( 'NONE', #11391, #4565, #8476 ) ;
#10231 = MANIFOLD_SOLID_BREP ( 'Hex', #4371 ) ;
#10232 = DIRECTION ( 'NONE',  ( 0.000000000000000000, -0.3513748240813304724, -0.9362348706397417564 ) ) ;
#10233 = DIRECTION ( 'NONE',  ( 1.000000000000000000, 0.000000000000000000, 0.000000000000000000 ) ) ;
#10234 = EDGE_CURVE ( 'NONE', #4020, #12600, #661, .T. ) ;
#10235 = CARTESIAN_POINT ( 'NONE',  ( 9.000000000000017764, -12.49999999999999645, -1.576761677324507637E-16 ) ) ;
#10236 = B_SPLINE_CURVE_WITH_KNOTS ( 'NONE', 3,
 ( #3924, #7663, #1861, #11850, #11786, #4891, #10735, #5782 ),
 .UNSPECIFIED., .F., .F.,
 ( 4, 2, 2, 4 ),
 ( 2.465131517071101953E-07, 0.001183067374689835902, 0.001774477805458900314, 0.002365888236227965159 ),
 .UNSPECIFIED. ) ;
#10237 = EDGE_CURVE ( 'NONE', #3455, #1611, #11713, .T. ) ;
#10238 = CARTESIAN_POINT ( 'NONE',  ( 9.999999999999994671, -7.301715115245778875, 1.202063382601485042 ) ) ;
#10239 = FILL_AREA_STYLE ('',( #4340 ) ) ;
#10240 = CIRCLE ( 'NONE', #10064, 2.149999999999994138 ) ;
#10241 = CIRCLE ( 'NONE', #10665, 2.800000000000002931 ) ;
#10242 = VERTEX_POINT ( 'NONE', #5808 ) ;
#10243 = DIRECTION ( 'NONE',  ( 0.000000000000000000, 0.000000000000000000, -1.000000000000000000 ) ) ;
#10244 = ORIENTED_EDGE ( 'NONE', *, *, #2624, .T. ) ;
#10245 = CIRCLE ( 'NONE', #4717, 2.800000000000002487 ) ;
#10246 = ORIENTED_EDGE ( 'NONE', *, *, #217, .F. ) ;
#10247 = CONTEXT_DEPENDENT_SHAPE_REPRESENTATION ( #8958, #9840 ) ;
#10248 = VERTEX_POINT ( 'NONE', #8455 ) ;
#10249 = CARTESIAN_POINT ( 'NONE',  ( 40.00000000000006395, -4.499999999999998224, -20.00000000000000000 ) ) ;
#10250 = DIRECTION ( 'NONE',  ( 0.000000000000000000, 1.000000000000000000, 0.000000000000000000 ) ) ;
#10251 = CIRCLE ( 'NONE', #4091, 2.149999999999994138 ) ;
#10252 = FACE_OUTER_BOUND ( 'NONE', #902, .T. ) ;
#10253 = DIRECTION ( 'NONE',  ( 0.000000000000000000, 1.000000000000000000, 0.000000000000000000 ) ) ;
#10254 = CIRCLE ( 'NONE', #8626, 1.535500000000001863 ) ;
#10255 = AXIS2_PLACEMENT_3D ( 'NONE', #10300, #8978, #161 ) ;
#10256 = DIRECTION ( 'NONE',  ( 7.821394097150993714E-30, 0.8660254037844392627, 0.4999999999999991673 ) ) ;
#10257 = ORIENTED_EDGE ( 'NONE', *, *, #3994, .F. ) ;
#10258 = FACE_OUTER_BOUND ( 'NONE', #12316, .T. ) ;
#10259 = AXIS2_PLACEMENT_3D ( 'NONE', #2791, #7066, #6644 ) ;
#10260 = ADVANCED_FACE ( 'NONE', ( #10636 ), #12524, .T. ) ;
#10261 = CYLINDRICAL_SURFACE ( 'NONE', #5754, 3.999999999999997335 ) ;
#10262 = ORIENTED_EDGE ( 'NONE', *, *, #2067, .F. ) ;
#10263 = ORIENTED_EDGE ( 'NONE', *, *, #11543, .T. ) ;
#10264 = ORIENTED_EDGE ( 'NONE', *, *, #4683, .F. ) ;
#10265 = AXIS2_PLACEMENT_3D ( 'NONE', #9703, #12635, #10869 ) ;
#10266 = ORIENTED_EDGE ( 'NONE', *, *, #3140, .F. ) ;
#10267 = CIRCLE ( 'NONE', #3104, 2.800000000000003375 ) ;
#10268 = CIRCLE ( 'NONE', #2482, 4.499999999999999112 ) ;
#10269 = DIRECTION ( 'NONE',  ( 0.000000000000000000, 0.000000000000000000, -1.000000000000000000 ) ) ;
#10270 = EDGE_CURVE ( 'NONE', #6684, #4187, #10254, .T. ) ;
#10271 = PRODUCT ( 'Serrated Eccentric Cam Pawl', 'Serrated Eccentric Cam Pawl', '', ( #9805 ) ) ;
#10272 = DIRECTION ( 'NONE',  ( 1.000000000000000000, 0.000000000000000000, 0.000000000000000000 ) ) ;
#10273 = ORIENTED_EDGE ( 'NONE', *, *, #7229, .F. ) ;
#10274 =( REPRESENTATION_RELATIONSHIP ('NONE','NONE', #10018, #9199 ) REPRESENTATION_RELATIONSHIP_WITH_TRANSFORMATION ( #4278 )SHAPE_REPRESENTATION_RELATIONSHIP( ) );
#10275 = CARTESIAN_POINT ( 'NONE',  ( 19.99999999999999645, 4.494880553659021061, 4.802513683199234329 ) ) ;
#10276 = ORIENTED_EDGE ( 'NONE', *, *, #12307, .T. ) ;
#10277 = LINE ( 'NONE', #7652, #4479 ) ;
#10278 = CARTESIAN_POINT ( 'NONE',  ( -35.00000000000006395, 30.00000000000000000, 2.000000000000007994 ) ) ;
#10279 =( GEOMETRIC_REPRESENTATION_CONTEXT ( 3 ) GLOBAL_UNCERTAINTY_ASSIGNED_CONTEXT ( ( #1818 ) ) GLOBAL_UNIT_ASSIGNED_CONTEXT ( ( #8735, #1233, #2896 ) ) REPRESENTATION_CONTEXT ( 'NONE', 'WORKASPACE' ) );
#10280 = VECTOR ( 'NONE', #10538, 1000.000000000000000 ) ;
#10281 = EDGE_CURVE ( 'NONE', #3923, #6222, #6985, .T. ) ;
#10282 = FACE_OUTER_BOUND ( 'NONE', #6999, .T. ) ;
#10283 = ADVANCED_FACE ( 'NONE', ( #9660 ), #10447, .T. ) ;
#10284 = CARTESIAN_POINT ( 'NONE',  ( 19.99999999999999645, -4.155687294075622873, 5.098857909653524700 ) ) ;
#10285 = ORIENTED_EDGE ( 'NONE', *, *, #5572, .T. ) ;
#10286 = ORIENTED_EDGE ( 'NONE', *, *, #5796, .T. ) ;
#10287 = DIRECTION ( 'NONE',  ( -1.000000000000000000, 0.000000000000000000, 2.017120320903271344E-16 ) ) ;
#10288 = EDGE_CURVE ( 'NONE', #3836, #9690, #5622, .T. ) ;
#10289 =( LENGTH_UNIT ( ) NAMED_UNIT ( * ) SI_UNIT ( .MILLI., .METRE. ) );
#10290 = CARTESIAN_POINT ( 'NONE',  ( -4.198928548860765275, 0.8158838809860013974, -3.526471437616931937 ) ) ;
#10291 = DIRECTION ( 'NONE',  ( 0.000000000000000000, 0.000000000000000000, 1.000000000000000000 ) ) ;
#10292 = CARTESIAN_POINT ( 'NONE',  ( 0.000000000000000000, 7.164568425986757916, 1.851744925564474675 ) ) ;
#10293 = CARTESIAN_POINT ( 'NONE',  ( 9.999999999999998224, -1.113123845672307155, -7.315801754025040182 ) ) ;
#10294 = AXIS2_PLACEMENT_3D ( 'NONE', #7055, #2159, #3208 ) ;
#10295 = DIRECTION ( 'NONE',  ( -1.000000000000000000, 0.000000000000000000, 0.000000000000000000 ) ) ;
#10296 = ORIENTED_EDGE ( 'NONE', *, *, #4328, .F. ) ;
#10297 = CARTESIAN_POINT ( 'NONE',  ( 1.274258131565028762, 3.883108878240869810, -3.220599429844238415 ) ) ;
#10298 = CARTESIAN_POINT ( 'NONE',  ( 33.00000000000001421, 39.34792583643766761, -14.56347054209569158 ) ) ;
#10299 =( LENGTH_UNIT ( ) NAMED_UNIT ( * ) SI_UNIT ( .MILLI., .METRE. ) );
#10300 = CARTESIAN_POINT ( 'NONE',  ( 2.000000000000001776, 0.000000000000000000, 0.000000000000000000 ) ) ;
#10301 = CIRCLE ( 'NONE', #1480, 4.000000000000000000 ) ;
#10302 = ORIENTED_EDGE ( 'NONE', *, *, #5301, .T. ) ;
#10303 = CARTESIAN_POINT ( 'NONE',  ( 0.000000000000000000, -3.730839900301574197, 5.321450426182483540 ) ) ;
#10304 = DIRECTION ( 'NONE',  ( 0.000000000000000000, -0.5128992774058949156, -0.8584487936018728726 ) ) ;
#10305 = LINE ( 'NONE', #1561, #6112 ) ;
#10306 = DIRECTION ( 'NONE',  ( -1.000000000000000000, 1.006188713385347367E-17, 3.844790828812615713E-17 ) ) ;
#10307 = DIRECTION ( 'NONE',  ( 0.000000000000000000, -0.000000000000000000, 1.000000000000000000 ) ) ;
#10308 = CARTESIAN_POINT ( 'NONE',  ( 11.00000000000003375, -3.490243377569932395E-16, 22.15000000000003411 ) ) ;
#10309 = VECTOR ( 'NONE', #6713, 1000.000000000000000 ) ;
#10310 = DIRECTION ( 'NONE',  ( -1.000000000000000000, 1.010728034814421376E-30, 1.090846720500930387E-30 ) ) ;
#10311 = ORIENTED_EDGE ( 'NONE', *, *, #11321, .F. ) ;
#10312 = DIRECTION ( 'NONE',  ( -1.000000000000000000, 1.010728034814421376E-30, 1.090846720500930387E-30 ) ) ;
#10313 = ORIENTED_EDGE ( 'NONE', *, *, #1226, .F. ) ;
#10314 = ITEM_DEFINED_TRANSFORMATION ( 'NONE', 'NONE', #9995,  #12422 ) ;
#10315 = ADVANCED_FACE ( 'NONE', ( #6538 ), #8584, .T. ) ;
#10316 = ORIENTED_EDGE ( 'NONE', *, *, #8874, .F. ) ;
#10317 = ORIENTED_EDGE ( 'NONE', *, *, #9331, .F. ) ;
#10318 = CIRCLE ( 'NONE', #12207, 6.499000000000008548 ) ;
#10319 = CYLINDRICAL_SURFACE ( 'NONE', #2129, 2.149999999999999023 ) ;
#10320 = VECTOR ( 'NONE', #3795, 1000.000000000000000 ) ;
#10321 = DIRECTION ( 'NONE',  ( -1.031065855027150586E-29, 1.000000000000000000, -1.779758311459930984E-16 ) ) ;
#10322 = CYLINDRICAL_SURFACE ( 'NONE', #5723, 2.800000000000003819 ) ;
#10323 = DIRECTION ( 'NONE',  ( -1.000000000000000000, 1.006188713385347367E-17, 3.844790828812615713E-17 ) ) ;
#10324 = ORIENTED_EDGE ( 'NONE', *, *, #9338, .F. ) ;
#10325 = CARTESIAN_POINT ( 'NONE',  ( 4.198928548860774157, -0.8158838809860118335, -3.526471437616922167 ) ) ;
#10326 = DIRECTION ( 'NONE',  ( 0.000000000000000000, -1.000000000000000000, 0.000000000000000000 ) ) ;
#10327 = EDGE_LOOP ( 'NONE', ( #11357, #8990, #7450, #7056 ) ) ;
#10328 = AXIS2_PLACEMENT_3D ( 'NONE', #5193, #3278, #7191 ) ;
#10329 = ORIENTED_EDGE ( 'NONE', *, *, #9722, .T. ) ;
#10330 = CIRCLE ( 'NONE', #4794, 6.000000000000013323 ) ;
#10331 = CARTESIAN_POINT ( 'NONE',  ( 19.99999999999999645, 4.596015818000074304, 4.705818469689523553 ) ) ;
#10332 = ORIENTED_EDGE ( 'NONE', *, *, #2405, .F. ) ;
#10333 = AXIS2_PLACEMENT_3D ( 'NONE', #6293, #12103, #3230 ) ;
#10334 = ORIENTED_EDGE ( 'NONE', *, *, #8637, .T. ) ;
#10335 = FILL_AREA_STYLE ('',( #7515 ) ) ;
#10336 = ADVANCED_FACE ( 'NONE', ( #2007, #10757 ), #7869, .F. ) ;
#10337 = FILL_AREA_STYLE ('',( #12233 ) ) ;
#10338 = VERTEX_POINT ( 'NONE', #7037 ) ;
#10339 = DIRECTION ( 'NONE',  ( 1.000000000000000000, 1.031065855027150586E-29, -2.218671295934095703E-30 ) ) ;
#10340 = DIRECTION ( 'NONE',  ( 0.000000000000000000, 5.551115123125777155E-17, 1.000000000000000000 ) ) ;
#10341 = ORIENTED_EDGE ( 'NONE', *, *, #4685, .F. ) ;
#10342 = VECTOR ( 'NONE', #7441, 1000.000000000000000 ) ;
#10343 = DIRECTION ( 'NONE',  ( -1.000000000000000000, 1.010728034814421376E-30, 1.090846720500930387E-30 ) ) ;
#10344 = CARTESIAN_POINT ( 'NONE',  ( -0.3461262719736130089, 4.658553426539255859, -3.671615880910391816 ) ) ;
#10345 = DIRECTION ( 'NONE',  ( -1.000000000000000000, 0.000000000000000000, 0.000000000000000000 ) ) ;
#10346 = UNCERTAINTY_MEASURE_WITH_UNIT (LENGTH_MEASURE( 1.000000000000000082E-05 ), #11284, 'distance_accuracy_value', 'NONE');
#10347 = CARTESIAN_POINT ( 'NONE',  ( 33.00000000000001421, 81.84122341717352356, -27.68198508464163510 ) ) ;
#10348 = ORIENTED_EDGE ( 'NONE', *, *, #8917, .F. ) ;
#10349 = AXIS2_PLACEMENT_3D ( 'NONE', #9065, #4243, #10084 ) ;
#10350 = ORIENTED_EDGE ( 'NONE', *, *, #6738, .T. ) ;
#10351 = EDGE_CURVE ( 'NONE', #2985, #6306, #79, .T. ) ;
#10352 = CARTESIAN_POINT ( 'NONE',  ( 20.00000000000000000, 10.63631887905125950, -9.927230231572497843 ) ) ;
#10353 = EDGE_CURVE ( 'NONE', #3861, #9120, #9427, .T. ) ;
#10354 = DIRECTION ( 'NONE',  ( 7.038118388768703491E-30, 0.4999999999999988898, -0.8660254037844392627 ) ) ;
#10355 = ADVANCED_FACE ( 'NONE', ( #11873 ), #3882, .T. ) ;
#10356 = VECTOR ( 'NONE', #8582, 1000.000000000000000 ) ;
#10357 = DIRECTION ( 'NONE',  ( 2.187388225841179596E-16, -0.9997704357740726522, -0.02142605311579142552 ) ) ;
#10358 = VECTOR ( 'NONE', #5019, 1000.000000000000000 ) ;
#10359 = CARTESIAN_POINT ( 'NONE',  ( 40.00000000000006395, 2.500000000000000000, -20.00000000000000000 ) ) ;
#10360 = EDGE_CURVE ( 'NONE', #4950, #7142, #5996, .T. ) ;
#10361 = CARTESIAN_POINT ( 'NONE',  ( 19.99999999999999645, 0.000000000000000000, 0.000000000000000000 ) ) ;
#10362 = DIRECTION ( 'NONE',  ( -1.000000000000000000, 1.010728034814421376E-30, 1.090846720500930387E-30 ) ) ;
#10363 = ORIENTED_EDGE ( 'NONE', *, *, #3672, .T. ) ;
#10364 = CARTESIAN_POINT ( 'NONE',  ( 0.000000000000000000, -3.426907987218851481, 5.522074125465508132 ) ) ;
#10365 = CARTESIAN_POINT ( 'NONE',  ( -17.00000000000000000, 0.000000000000000000, 20.00000000000007461 ) ) ;
#10366 = ADVANCED_FACE ( 'NONE', ( #8050 ), #1943, .T. ) ;
#10367 = EDGE_CURVE ( 'NONE', #3527, #2170, #9648, .T. ) ;
#10368 = CARTESIAN_POINT ( 'NONE',  ( 20.00000000000000355, 18.52447679111067913, -16.77732469694377926 ) ) ;
#10369 = ORIENTED_EDGE ( 'NONE', *, *, #5077, .F. ) ;
#10370 = DIRECTION ( 'NONE',  ( 1.000000000000000000, 1.081682119347366321E-16, -6.938893903907228378E-17 ) ) ;
#10371 = CARTESIAN_POINT ( 'NONE',  ( 40.00000000000000711, 10.26855730552414059, -22.42000078613342851 ) ) ;
#10373 = CARTESIAN_POINT ( 'NONE',  ( 34.00000000000000000, 1.971681346627238735E-16, -1.610000000000017417 ) ) ;
#10372 = AXIS2_PLACEMENT_3D ( 'NONE', #6046, #11913, #7152 ) ;
#10374 = CARTESIAN_POINT ( 'NONE',  ( 4.024499207728855055, -2.323545700935701674, -3.572172305156885219 ) ) ;
#10375 = AXIS2_PLACEMENT_3D ( 'NONE', #2306, #233, #4418 ) ;
#10376 = CARTESIAN_POINT ( 'NONE',  ( 14.00000000000000000, 30.00000000000000000, 0.000000000000000000 ) ) ;
#10377 = DIRECTION ( 'NONE',  ( -1.000000000000000000, 0.000000000000000000, 0.000000000000000000 ) ) ;
#10378 = DIRECTION ( 'NONE',  ( 7.038118388768703491E-30, 0.4999999999999988898, -0.8660254037844392627 ) ) ;
#10379 = DIRECTION ( 'NONE',  ( 0.000000000000000000, 0.000000000000000000, 1.000000000000000000 ) ) ;
#10380 = VERTEX_POINT ( 'NONE', #4912 ) ;
#10381 = EDGE_CURVE ( 'NONE', #291, #7883, #2267, .T. ) ;
#10382 = AXIS2_PLACEMENT_3D ( 'NONE', #8906, #7585, #1050 ) ;
#10383 = AXIS2_PLACEMENT_3D ( 'NONE', #12589, #4466, #12332 ) ;
#10384 = ORIENTED_EDGE ( 'NONE', *, *, #12170, .T. ) ;
#10385 = VERTEX_POINT ( 'NONE', #7807 ) ;
#10386 = EDGE_CURVE ( 'NONE', #11433, #11940, #4736, .T. ) ;
#10387 = DIRECTION ( 'NONE',  ( -1.000000000000000000, 1.010728034814421376E-30, 1.090846720500930387E-30 ) ) ;
#10388 = CARTESIAN_POINT ( 'NONE',  ( 27.00000000000001421, 39.34792583643766761, -24.06347054209567915 ) ) ;
#10389 = LINE ( 'NONE', #8591, #8629 ) ;
#10390 = CARTESIAN_POINT ( 'NONE',  ( 19.99999999999999645, -5.774092856145700559, -2.982759240804946810 ) ) ;
#10391 = ORIENTED_EDGE ( 'NONE', *, *, #4980, .T. ) ;
#10392 = EDGE_CURVE ( 'NONE', #9681, #11065, #2139, .T. ) ;
#10393 = FACE_OUTER_BOUND ( 'NONE', #10649, .T. ) ;
#10394 = AXIS2_PLACEMENT_3D ( 'NONE', #1545, #11346, #2658 ) ;
#10395 = LINE ( 'NONE', #1580, #5561 ) ;
#10396 = VERTEX_POINT ( 'NONE', #4976 ) ;
#10397 = ORIENTED_EDGE ( 'NONE', *, *, #12352, .F. ) ;
#10398 = FACE_OUTER_BOUND ( 'NONE', #9175, .T. ) ;
#10399 = ORIENTED_EDGE ( 'NONE', *, *, #6391, .T. ) ;
#10400 = EDGE_LOOP ( 'NONE', ( #12555, #8290 ) ) ;
#10401 =( NAMED_UNIT ( * ) PLANE_ANGLE_UNIT ( ) SI_UNIT ( $, .RADIAN. ) );
#10402 = VERTEX_POINT ( 'NONE', #2998 ) ;
#10403 = ADVANCED_FACE ( 'NONE', ( #9847 ), #1037, .T. ) ;
#10404 = DIRECTION ( 'NONE',  ( 1.000000000000000000, -0.000000000000000000, -6.938893903907228378E-17 ) ) ;
#10405 = AXIS2_PLACEMENT_3D ( 'NONE', #421, #4414, #4224 ) ;
#10406 = LINE ( 'NONE', #8291, #799 ) ;
#10407 = ORIENTED_EDGE ( 'NONE', *, *, #12538, .T. ) ;
#10408 = LINE ( 'NONE', #1594, #9806 ) ;
#10409 = DIRECTION ( 'NONE',  ( -1.000000000000000000, 1.010728034814421376E-30, 1.090846720500930387E-30 ) ) ;
#10410 = EDGE_CURVE ( 'NONE', #10811, #825, #11935, .T. ) ;
#10411 = CARTESIAN_POINT ( 'NONE',  ( 15.00000000000003375, 30.00000000000001776, 4.000000000000008882 ) ) ;
#10412 = EDGE_CURVE ( 'NONE', #4937, #10180, #10687, .T. ) ;
#10413 = B_SPLINE_CURVE_WITH_KNOTS ( 'NONE', 3,
 ( #11000, #7144, #8997, #6041, #10081, #3100, #10206, #5145 ),
 .UNSPECIFIED., .F., .F.,
 ( 4, 2, 2, 4 ),
 ( 0.005725059856848646080, 0.006314084072593635286, 0.006903108288338623624, 0.008081156719828602036 ),
 .UNSPECIFIED. ) ;
#10414 = EDGE_CURVE ( 'NONE', #7570, #8231, #9849, .T. ) ;
#10415 = AXIS2_PLACEMENT_3D ( 'NONE', #9010, #4256, #8113 ) ;
#10416 = CYLINDRICAL_SURFACE ( 'NONE', #831, 2.800000000000003819 ) ;
#10417 = EDGE_CURVE ( 'NONE', #3527, #4184, #12000, .T. ) ;
#10418 = CIRCLE ( 'NONE', #1162, 0.2000000000000000944 ) ;
#10419 = ORIENTED_EDGE ( 'NONE', *, *, #1838, .T. ) ;
#10420 = ORIENTED_EDGE ( 'NONE', *, *, #10627, .T. ) ;
#10421 = DIRECTION ( 'NONE',  ( -1.000000000000000000, -1.081682119347366197E-16, 6.938893903907228378E-17 ) ) ;
#10422 = DIRECTION ( 'NONE',  ( -1.000000000000000000, -1.081682119347362869E-16, 3.143182988685428759E-16 ) ) ;
#10423 = EDGE_LOOP ( 'NONE', ( #3347, #6893, #1012, #1504 ) ) ;
#10424 = CARTESIAN_POINT ( 'NONE',  ( -2.775557561562891351E-14, -4.618802153517012954, -0.5000000000000004441 ) ) ;
#10425 = AXIS2_PLACEMENT_3D ( 'NONE', #11594, #4639, #8558 ) ;
#10426 = DIRECTION ( 'NONE',  ( 1.000000000000000000, 0.000000000000000000, -2.168404344971007882E-16 ) ) ;
#10427 = CIRCLE ( 'NONE', #1791, 6.499000000000008548 ) ;
#10428 = CARTESIAN_POINT ( 'NONE',  ( 2.000000000000091926, 0.8865213383406691516, -1.535500000000002085 ) ) ;
#10429 = EDGE_CURVE ( 'NONE', #12605, #6210, #12717, .T. ) ;
#10430 = CARTESIAN_POINT ( 'NONE',  ( 9.757359312880696578, 30.00000000000000000, -4.242640687119267007 ) ) ;
#10431 = ORIENTED_EDGE ( 'NONE', *, *, #254, .F. ) ;
#10432 = CARTESIAN_POINT ( 'NONE',  ( -0.1756481739660440966, 4.720212674038974932, -3.469390959564073285 ) ) ;
#10433 = AXIS2_PLACEMENT_3D ( 'NONE', #3789, #1910, #11703 ) ;
#10434 = CARTESIAN_POINT ( 'NONE',  ( 0.000000000000000000, 0.000000000000000000, 0.000000000000000000 ) ) ;
#10435 = SURFACE_STYLE_USAGE ( .BOTH. , #2596 ) ;
#10436 = EDGE_CURVE ( 'NONE', #6015, #3764, #405, .T. ) ;
#10437 = DIRECTION ( 'NONE',  ( -1.000000000000000000, 1.010728034814421376E-30, 1.090846720500930387E-30 ) ) ;
#10438 = ORIENTED_EDGE ( 'NONE', *, *, #11338, .T. ) ;
#10439 = CARTESIAN_POINT ( 'NONE',  ( 20.00000000000006750, -8.724036641233686229E-16, -20.00000000000000000 ) ) ;
#10440 = DIRECTION ( 'NONE',  ( 4.606824426974262030E-31, 0.5128992774059070170, -0.8584487936018656562 ) ) ;
#10441 = CARTESIAN_POINT ( 'NONE',  ( 1.654252653721900224, 3.663718938583006235, -0.01223254789872770323 ) ) ;
#10442 = CYLINDRICAL_SURFACE ( 'NONE', #4671, 24.99999999999999289 ) ;
#10443 = CARTESIAN_POINT ( 'NONE',  ( 4.000000000000003553, 0.000000000000000000, 3.500000000000000000 ) ) ;
#10444 = ADVANCED_FACE ( 'NONE', ( #1293 ), #6319, .F. ) ;
#10445 = CARTESIAN_POINT ( 'NONE',  ( 19.99999999999999645, -5.774092856145738750, 2.982759240804856660 ) ) ;
#10446 = EDGE_CURVE ( 'NONE', #4508, #5455, #7413, .T. ) ;
#10447 = CYLINDRICAL_SURFACE ( 'NONE', #3095, 2.800000000000003819 ) ;
#10448 = UNCERTAINTY_MEASURE_WITH_UNIT (LENGTH_MEASURE( 1.000000000000000082E-05 ), #6131, 'distance_accuracy_value', 'NONE');
#10449 = DIRECTION ( 'NONE',  ( 0.000000000000000000, 0.000000000000000000, 1.000000000000000000 ) ) ;
#10450 = ORIENTED_EDGE ( 'NONE', *, *, #4338, .T. ) ;
#10451 = CONICAL_SURFACE ( 'NONE', #6346, 4.000000000000000000, 0.8911886515913786111 ) ;
#10452 = EDGE_LOOP ( 'NONE', ( #685, #2400 ) ) ;
#10453 = ORIENTED_EDGE ( 'NONE', *, *, #7577, .T. ) ;
#10454 = CARTESIAN_POINT ( 'NONE',  ( 9.000000000000017764, 19.99999999999999645, 9.850000000000029843 ) ) ;
#10455 = CARTESIAN_POINT ( 'NONE',  ( 19.99999999999999645, -4.999339924971576643, 4.274890546383965706 ) ) ;
#10456 = CARTESIAN_POINT ( 'NONE',  ( 2.000000000000001776, 0.000000000000000000, 0.000000000000000000 ) ) ;
#10457 = DIRECTION ( 'NONE',  ( -1.000000000000000000, 1.010728034814421376E-30, 1.090846720500930387E-30 ) ) ;
#10458 = EDGE_LOOP ( 'NONE', ( #6486, #10974, #11327, #3522 ) ) ;
#10459 = CARTESIAN_POINT ( 'NONE',  ( 0.000000000000000000, -0.8732627748487655772, -7.348293143721449816 ) ) ;
#10460 = VECTOR ( 'NONE', #12543, 1000.000000000000000 ) ;
#10461 = CIRCLE ( 'NONE', #1216, 2.800000000000003375 ) ;
#10462 = ORIENTED_EDGE ( 'NONE', *, *, #11872, .T. ) ;
#10463 = ORIENTED_EDGE ( 'NONE', *, *, #11605, .F. ) ;
#10464 = LINE ( 'NONE', #1649, #11506 ) ;
#10465 = EDGE_LOOP ( 'NONE', ( #1669, #10114, #9817, #3459 ) ) ;
#10466 = ORIENTED_EDGE ( 'NONE', *, *, #6576, .T. ) ;
#10467 = EDGE_CURVE ( 'NONE', #1153, #4528, #8314, .T. ) ;
#10468 = B_SPLINE_CURVE_WITH_KNOTS ( 'NONE', 3,
 ( #11612, #10507, #11739, #10754, #11675, #3696, #9656, #10693 ),
 .UNSPECIFIED., .F., .F.,
 ( 4, 2, 2, 4 ),
 ( 0.000000000000000000, 0.002450665683189820129, 0.003675998524784730194, 0.004901331366379640259 ),
 .UNSPECIFIED. ) ;
#10469 = AXIS2_PLACEMENT_3D ( 'NONE', #7478, #12315, #9328 ) ;
#10471 = AXIS2_PLACEMENT_3D ( 'NONE', #12427, #2639, #4367 ) ;
#10470 =( NAMED_UNIT ( * ) PLANE_ANGLE_UNIT ( ) SI_UNIT ( $, .RADIAN. ) );
#10472 = MECHANICAL_DESIGN_GEOMETRIC_PRESENTATION_REPRESENTATION (  '', ( #12336 ), #5337 ) ;
#10473 = EDGE_LOOP ( 'NONE', ( #410, #4137, #252, #9093 ) ) ;
#10474 = DIRECTION ( 'NONE',  ( 0.000000000000000000, 0.000000000000000000, 1.000000000000000000 ) ) ;
#10475 = CARTESIAN_POINT ( 'NONE',  ( 2.000000000000001776, 1.773042676681341856, -3.469446951953614189E-15 ) ) ;
#10476 = ORIENTED_EDGE ( 'NONE', *, *, #7236, .F. ) ;
#10477 = CARTESIAN_POINT ( 'NONE',  ( -2.775557561562891351E-14, -4.618802153517012954, -0.5000000000000004441 ) ) ;
#10478 = DIRECTION ( 'NONE',  ( 0.000000000000000000, 0.9989930665413144784, 0.04486483035051876817 ) ) ;
#10479 = CYLINDRICAL_SURFACE ( 'NONE', #7105, 6.499000000000010324 ) ;
#10480 = AXIS2_PLACEMENT_3D ( 'NONE', #1987, #11662, #5858 ) ;
#10481 = UNCERTAINTY_MEASURE_WITH_UNIT (LENGTH_MEASURE( 1.000000000000000082E-05 ), #3192, 'distance_accuracy_value', 'NONE');
#10482 = CIRCLE ( 'NONE', #5151, 7.400000000000009237 ) ;
#10483 = CIRCLE ( 'NONE', #7610, 2.800000000000003375 ) ;
#10484 = ORIENTED_EDGE ( 'NONE', *, *, #3201, .T. ) ;
#10485 = VERTEX_POINT ( 'NONE', #12194 ) ;
#10486 = CARTESIAN_POINT ( 'NONE',  ( 40.00000000000000711, 8.524476791110680907, -16.77732469694377926 ) ) ;
#10487 = CARTESIAN_POINT ( 'NONE',  ( 0.000000000000000000, 0.000000000000000000, 0.000000000000000000 ) ) ;
#10488 = ORIENTED_EDGE ( 'NONE', *, *, #11189, .F. ) ;
#10489 = ADVANCED_FACE ( 'NONE', ( #12257 ), #330, .T. ) ;
#10490 = LINE ( 'NONE', #1735, #9426 ) ;
#10491 = AXIS2_PLACEMENT_3D ( 'NONE', #12290, #12226, #11381 ) ;
#10492 = EDGE_CURVE ( 'NONE', #7234, #11776, #1020, .T. ) ;
#10493 = AXIS2_PLACEMENT_3D ( 'NONE', #5792, #67, #11919 ) ;
#10494 = VECTOR ( 'NONE', #10689, 1000.000000000000000 ) ;
#10495 = DIRECTION ( 'NONE',  ( -1.000000000000000000, 1.010728034814421376E-30, 1.090846720500930387E-30 ) ) ;
#10496 = DIRECTION ( 'NONE',  ( 1.000000000000000000, 1.081682119347366321E-16, -6.938893903907228378E-17 ) ) ;
#10497 = DIRECTION ( 'NONE',  ( 1.140150527077241873E-30, 0.000000000000000000, -1.000000000000000000 ) ) ;
#10498 = VERTEX_POINT ( 'NONE', #1229 ) ;
#10499 = CARTESIAN_POINT ( 'NONE',  ( 0.000000000000000000, -4.618802153517027165, -5.000000000000000888 ) ) ;
#10500 = CARTESIAN_POINT ( 'NONE',  ( 11.00000000000001599, 19.99999999999999645, 9.850000000000029843 ) ) ;
#10501 = DIRECTION ( 'NONE',  ( 0.000000000000000000, 0.000000000000000000, 1.000000000000000000 ) ) ;
#10502 = EDGE_CURVE ( 'NONE', #3764, #10396, #9042, .T. ) ;
#10503 = DIRECTION ( 'NONE',  ( -1.000000000000000000, -1.081682119347366197E-16, 6.938893903907228378E-17 ) ) ;
#10504 = LINE ( 'NONE', #11912, #6459 ) ;
#10505 = PRESENTATION_LAYER_ASSIGNMENT (  '', '', ( #7628 ) ) ;
#10506 = DIRECTION ( 'NONE',  ( -1.000000000000000000, 1.010728034814421376E-30, 1.090846720500930387E-30 ) ) ;
#10507 = CARTESIAN_POINT ( 'NONE',  ( 3.511755186886750923, -2.826662030176405160, -3.597382984111576754 ) ) ;
#10508 = DIRECTION ( 'NONE',  ( -1.000000000000000000, 1.010728034814421376E-30, 1.090846720500930387E-30 ) ) ;
#10509 = CARTESIAN_POINT ( 'NONE',  ( -11.83215956619923226, -30.00000000000000000, 2.000000000000000000 ) ) ;
#10510 = DIRECTION ( 'NONE',  ( 0.000000000000000000, 0.000000000000000000, 1.000000000000000000 ) ) ;
#10511 = DIRECTION ( 'NONE',  ( 0.000000000000000000, 0.000000000000000000, 1.000000000000000000 ) ) ;
#10512 = ORIENTED_EDGE ( 'NONE', *, *, #4682, .T. ) ;
#10513 = AXIS2_PLACEMENT_3D ( 'NONE', #8911, #2293, #9868 ) ;
#10514 = EDGE_CURVE ( 'NONE', #8559, #5751, #10267, .T. ) ;
#10515 = ORIENTED_EDGE ( 'NONE', *, *, #1262, .T. ) ;
#10516 = EDGE_CURVE ( 'NONE', #7272, #1057, #9208, .T. ) ;
#10517 = ORIENTED_EDGE ( 'NONE', *, *, #5923, .T. ) ;
#10518 = DIRECTION ( 'NONE',  ( 1.000000000000000000, -0.000000000000000000, -6.938893903907228378E-17 ) ) ;
#10519 = EDGE_CURVE ( 'NONE', #8354, #9064, #11937, .T. ) ;
#10520 = CARTESIAN_POINT ( 'NONE',  ( 0.1999999999999987899, 0.000000000000000000, -1.734723475976807094E-14 ) ) ;
#10521 = CARTESIAN_POINT ( 'NONE',  ( 15.00000000000003375, 30.00000000000001776, -9.742497179615118866E-31 ) ) ;
#10522 = DIRECTION ( 'NONE',  ( -1.000000000000000000, -1.081682119347366197E-16, 6.938893903907228378E-17 ) ) ;
#10523 = ORIENTED_EDGE ( 'NONE', *, *, #11922, .F. ) ;
#10524 = FACE_BOUND ( 'NONE', #12542, .T. ) ;
#10525 = VECTOR ( 'NONE', #2078, 1000.000000000000000 ) ;
#10526 = ADVANCED_FACE ( 'NONE', ( #2401 ), #3498, .F. ) ;
#10527 = CARTESIAN_POINT ( 'NONE',  ( 11.17157287525379772, -12.99999999999999822, -2.828427124746177856 ) ) ;
#10528 = ORIENTED_EDGE ( 'NONE', *, *, #4701, .F. ) ;
#10529 = ORIENTED_EDGE ( 'NONE', *, *, #342, .F. ) ;
#10530 = CYLINDRICAL_SURFACE ( 'NONE', #4325, 7.400000000000010125 ) ;
#10531 = ORIENTED_EDGE ( 'NONE', *, *, #1305, .T. ) ;
#10532 = VERTEX_POINT ( 'NONE', #8117 ) ;
#10533 =( LENGTH_UNIT ( ) NAMED_UNIT ( * ) SI_UNIT ( .MILLI., .METRE. ) );
#10534 = VECTOR ( 'NONE', #9135, 1000.000000000000000 ) ;
#10535 = DIRECTION ( 'NONE',  ( -2.465190328815656418E-32, 1.177425296209236734E-30, 1.000000000000000000 ) ) ;
#10536 = ORIENTED_EDGE ( 'NONE', *, *, #5521, .T. ) ;
#10537 = CARTESIAN_POINT ( 'NONE',  ( 20.00000000000000000, 22.56100271565320625, -6.249672610153678143 ) ) ;
#10538 = DIRECTION ( 'NONE',  ( -1.000000000000000000, 1.010728034814421376E-30, 1.090846720500930387E-30 ) ) ;
#10539 = ORIENTED_EDGE ( 'NONE', *, *, #1660, .F. ) ;
#10540 = CARTESIAN_POINT ( 'NONE',  ( -27.85000000000000497, 2.632990618166804305E-16, 2.000000000000001332 ) ) ;
#10541 = CARTESIAN_POINT ( 'NONE',  ( 14.00000000000000000, 44.64000000000000057, -5.000000000000000888 ) ) ;
#10542 = AXIS2_PLACEMENT_3D ( 'NONE', #6133, #9978, #12068 ) ;
#10543 = AXIS2_PLACEMENT_3D ( 'NONE', #8490, #4764, #5599 ) ;
#10544 = ORIENTED_EDGE ( 'NONE', *, *, #8352, .F. ) ;
#10545 = VERTEX_POINT ( 'NONE', #3320 ) ;
#10546 = FACE_OUTER_BOUND ( 'NONE', #11272, .T. ) ;
#10547 = CIRCLE ( 'NONE', #6030, 2.100000000000000089 ) ;
#10548 = DIRECTION ( 'NONE',  ( -1.000000000000000000, 0.000000000000000000, -6.982962677686266711E-15 ) ) ;
#10549 = EDGE_LOOP ( 'NONE', ( #11369, #8788, #5658, #6426 ) ) ;
#10550 = LINE ( 'NONE', #12569, #2910 ) ;
#10551 = DIRECTION ( 'NONE',  ( -1.000000000000000000, 1.010728034814421376E-30, 1.090846720500930387E-30 ) ) ;
#10552 = EDGE_CURVE ( 'NONE', #8586, #1828, #4911, .T. ) ;
#10553 = CYLINDRICAL_SURFACE ( 'NONE', #10991, 2.100000000000000089 ) ;
#10554 = AXIS2_PLACEMENT_3D ( 'NONE', #337, #2474, #10440 ) ;
#10555 = DIRECTION ( 'NONE',  ( -1.000000000000000000, 1.010728034814421376E-30, 1.090846720500930387E-30 ) ) ;
#10556 = ORIENTED_EDGE ( 'NONE', *, *, #6206, .T. ) ;
#10557 = CARTESIAN_POINT ( 'NONE',  ( 19.99999999999999645, 0.000000000000000000, 0.000000000000000000 ) ) ;
#10558 = EDGE_LOOP ( 'NONE', ( #4242, #10763, #6117, #6955 ) ) ;
#10559 = DIRECTION ( 'NONE',  ( 0.000000000000000000, 1.177425296209237785E-30, 1.000000000000000000 ) ) ;
#10560 =( LENGTH_UNIT ( ) NAMED_UNIT ( * ) SI_UNIT ( .MILLI., .METRE. ) );
#10561 = DIRECTION ( 'NONE',  ( 1.000000000000000000, -1.010728034814421376E-30, -1.090846720500930387E-30 ) ) ;
#10562 = AXIS2_PLACEMENT_3D ( 'NONE', #2742, #8645, #8937 ) ;
#10563 = CARTESIAN_POINT ( 'NONE',  ( -18.00000000000002842, 30.00000000000000000, 4.336808689942017736E-16 ) ) ;
#10564 = CYLINDRICAL_SURFACE ( 'NONE', #5022, 2.800000000000003819 ) ;
#10565 = CARTESIAN_POINT ( 'NONE',  ( 0.000000000000000000, 0.000000000000000000, 0.000000000000000000 ) ) ;
#10566 = DIRECTION ( 'NONE',  ( 0.000000000000000000, 0.000000000000000000, 1.000000000000000000 ) ) ;
#10567 = DIRECTION ( 'NONE',  ( 0.000000000000000000, 0.000000000000000000, 1.000000000000000000 ) ) ;
#10568 = AXIS2_PLACEMENT_3D ( 'NONE', #723, #1815, #12462 ) ;
#10569 = DIRECTION ( 'NONE',  ( 0.000000000000000000, -1.000000000000000000, 0.000000000000000000 ) ) ;
#10570 = ADVANCED_FACE ( 'NONE', ( #1355 ), #12341, .F. ) ;
#10571 = EDGE_CURVE ( 'NONE', #8536, #10836, #8633, .T. ) ;
#10572 =( NAMED_UNIT ( * ) SI_UNIT ( $, .STERADIAN. ) SOLID_ANGLE_UNIT ( ) );
#10573 = B_SPLINE_CURVE_WITH_KNOTS ( 'NONE', 3,
 ( #12381, #2457, #10290, #3555, #4446, #641 ),
 .UNSPECIFIED., .F., .F.,
 ( 4, 2, 4 ),
 ( 0.002452478801916380645, 0.003676905084148010018, 0.004901331366379639391 ),
 .UNSPECIFIED. ) ;
#10574 = EDGE_CURVE ( 'NONE', #8669, #4937, #4706, .T. ) ;
#10575 = CARTESIAN_POINT ( 'NONE',  ( 19.99999999999999645, 1.834336845376711933, 6.234758161925244124 ) ) ;
#10576 = VERTEX_POINT ( 'NONE', #12388 ) ;
#10577 = CIRCLE ( 'NONE', #7100, 6.499000000000008548 ) ;
#10578 = EDGE_CURVE ( 'NONE', #8686, #2242, #5347, .T. ) ;
#10579 = ORIENTED_EDGE ( 'NONE', *, *, #8745, .T. ) ;
#10580 = CIRCLE ( 'NONE', #2376, 6.499000000000009436 ) ;
#10581 = ORIENTED_EDGE ( 'NONE', *, *, #12698, .T. ) ;
#10582 = CARTESIAN_POINT ( 'NONE',  ( -31.74999999999995026, 0.000000000000000000, -1.734723475976807094E-14 ) ) ;
#10583 = CARTESIAN_POINT ( 'NONE',  ( 19.99999999999999645, 0.000000000000000000, 0.000000000000000000 ) ) ;
#10584 = DIRECTION ( 'NONE',  ( -1.000000000000000000, -5.916456789157576279E-31, 1.224646799147353947E-16 ) ) ;
#10585 = CARTESIAN_POINT ( 'NONE',  ( 11.00000000000003375, -19.99999999999999645, 12.00000000000003553 ) ) ;
#10586 = ORIENTED_EDGE ( 'NONE', *, *, #6738, .F. ) ;
#10587 = DIRECTION ( 'NONE',  ( 1.000000000000000000, -1.010728034814421376E-30, -1.090846720500930387E-30 ) ) ;
#10588 = CARTESIAN_POINT ( 'NONE',  ( 19.99999999999999645, 0.000000000000000000, 0.000000000000000000 ) ) ;
#10589 = ORIENTED_EDGE ( 'NONE', *, *, #3792, .F. ) ;
#10590 = CIRCLE ( 'NONE', #9963, 2.800000000000002487 ) ;
#10591 = AXIS2_PLACEMENT_3D ( 'NONE', #10005, #3976, #6882 ) ;
#10592 = ORIENTED_EDGE ( 'NONE', *, *, #3514, .T. ) ;
#10593 = CARTESIAN_POINT ( 'NONE',  ( 14.00000000000000000, -13.00000000000000000, -6.000000000000001776 ) ) ;
#10594 = ORIENTED_EDGE ( 'NONE', *, *, #9225, .F. ) ;
#10595 = VERTEX_POINT ( 'NONE', #9519 ) ;
#10596 = DIRECTION ( 'NONE',  ( 0.000000000000000000, -0.8345732537213080837, 0.5508969814520944253 ) ) ;
#10597 = ORIENTED_EDGE ( 'NONE', *, *, #10977, .F. ) ;
#10598 = DIRECTION ( 'NONE',  ( 0.000000000000000000, 0.000000000000000000, -1.000000000000000000 ) ) ;
#10599 = EDGE_CURVE ( 'NONE', #6992, #10576, #8015, .T. ) ;
#10600 = DIRECTION ( 'NONE',  ( 0.000000000000000000, 0.6579387259397136978, -0.7530714660036098573 ) ) ;
#10601 = VERTEX_POINT ( 'NONE', #1806 ) ;
#10602 = AXIS2_PLACEMENT_3D ( 'NONE', #5300, #11232, #9216 ) ;
#10603 = DIRECTION ( 'NONE',  ( 1.000000000000000000, -0.000000000000000000, -6.938893903907228378E-17 ) ) ;
#10604 = DIRECTION ( 'NONE',  ( -1.000000000000000000, 1.006188713385347367E-17, 3.844790828812615713E-17 ) ) ;
#10605 = ORIENTED_EDGE ( 'NONE', *, *, #3927, .T. ) ;
#10606 = ADVANCED_FACE ( 'NONE', ( #4649 ), #5668, .T. ) ;
#10607 = EDGE_CURVE ( 'NONE', #11603, #1459, #10482, .T. ) ;
#10608 = ORIENTED_EDGE ( 'NONE', *, *, #8120, .T. ) ;
#10609 = VERTEX_POINT ( 'NONE', #11602 ) ;
#10610 = CARTESIAN_POINT ( 'NONE',  ( 2.000000000000001776, 0.000000000000000000, 0.000000000000000000 ) ) ;
#10611 = MECHANICAL_DESIGN_GEOMETRIC_PRESENTATION_REPRESENTATION (  '', ( #1772 ), #8959 ) ;
#10612 = DIRECTION ( 'NONE',  ( 3.143182988685428759E-16, -1.081682119347362623E-16, 1.000000000000000000 ) ) ;
#10613 = ORIENTED_EDGE ( 'NONE', *, *, #12183, .T. ) ;
#10614 = CYLINDRICAL_SURFACE ( 'NONE', #10043, 2.499999999999990230 ) ;
#10615 = DIRECTION ( 'NONE',  ( 0.000000000000000000, -1.530455820933490821E-32, 1.000000000000000000 ) ) ;
#10616 = VECTOR ( 'NONE', #737, 1000.000000000000000 ) ;
#10617 =( GEOMETRIC_REPRESENTATION_CONTEXT ( 3 ) GLOBAL_UNCERTAINTY_ASSIGNED_CONTEXT ( ( #2609 ) ) GLOBAL_UNIT_ASSIGNED_CONTEXT ( ( #1825, #8660, #3889 ) ) REPRESENTATION_CONTEXT ( 'NONE', 'WORKASPACE' ) );
#10618 = LINE ( 'NONE', #8876, #1539 ) ;
#10619 = EDGE_CURVE ( 'NONE', #1917, #6747, #9390, .T. ) ;
#10620 = CARTESIAN_POINT ( 'NONE',  ( 0.000000000000000000, 0.000000000000000000, 0.000000000000000000 ) ) ;
#10621 = VERTEX_POINT ( 'NONE', #10364 ) ;
#10622 = CARTESIAN_POINT ( 'NONE',  ( 2.000000000000001776, 1.773042676681341856, -3.469446951953614189E-15 ) ) ;
#10623 = ORIENTED_EDGE ( 'NONE', *, *, #11189, .T. ) ;
#10624 = CARTESIAN_POINT ( 'NONE',  ( 0.000000000000000000, 0.000000000000000000, 0.000000000000000000 ) ) ;
#10625 = CIRCLE ( 'NONE', #12496, 10.00000000000000178 ) ;
#10626 = CIRCLE ( 'NONE', #11260, 49.99999999999994316 ) ;
#10627 = EDGE_CURVE ( 'NONE', #6222, #10532, #3909, .T. ) ;
#10628 = CARTESIAN_POINT ( 'NONE',  ( 0.000000000000000000, 0.000000000000000000, 0.000000000000000000 ) ) ;
#10629 = FACE_OUTER_BOUND ( 'NONE', #7396, .T. ) ;
#10630 = DIRECTION ( 'NONE',  ( -1.000000000000000000, 1.010728034814421376E-30, 1.090846720500930387E-30 ) ) ;
#10631 = CARTESIAN_POINT ( 'NONE',  ( 4.000000000000003553, 2.343373503925209768E-16, -3.500000000000000000 ) ) ;
#10632 = DIRECTION ( 'NONE',  ( -1.000000000000000000, 1.006188713385347367E-17, 3.844790828812615713E-17 ) ) ;
#10633 = LINE ( 'NONE', #6784, #7117 ) ;
#10634 = DIRECTION ( 'NONE',  ( 0.000000000000000000, 0.000000000000000000, 1.000000000000000000 ) ) ;
#10635 = VECTOR ( 'NONE', #295, 1000.000000000000000 ) ;
#10636 = FACE_OUTER_BOUND ( 'NONE', #1586, .T. ) ;
#10637 = CARTESIAN_POINT ( 'NONE',  ( 20.00000000000000000, 21.12780530657007461, -5.807015647486883481 ) ) ;
#10638 = EDGE_LOOP ( 'NONE', ( #4202, #3613, #3346, #12499 ) ) ;
#10639 = ORIENTED_EDGE ( 'NONE', *, *, #1820, .T. ) ;
#10640 = EDGE_CURVE ( 'NONE', #12228, #10862, #1230, .T. ) ;
#10641 = CARTESIAN_POINT ( 'NONE',  ( -30.00000000000000000, 30.00000000000000000, 0.000000000000000000 ) ) ;
#10642 = DIRECTION ( 'NONE',  ( 1.000000000000000000, 1.849040895279789448E-31, -6.938893903907224680E-17 ) ) ;
#10644 = EDGE_CURVE ( 'NONE', #6820, #4793, #3560, .T. ) ;
#10643 = DIRECTION ( 'NONE',  ( -1.000000000000000000, 1.010728034814421376E-30, 1.090846720500930387E-30 ) ) ;
#10645 = DIRECTION ( 'NONE',  ( 0.000000000000000000, 1.177425296209236909E-30, 1.000000000000000000 ) ) ;
#10646 = VERTEX_POINT ( 'NONE', #2663 ) ;
#10647 = FACE_OUTER_BOUND ( 'NONE', #12039, .T. ) ;
#10648 = ORIENTED_EDGE ( 'NONE', *, *, #3025, .F. ) ;
#10649 = EDGE_LOOP ( 'NONE', ( #3902, #4678, #675, #12701 ) ) ;
#10650 = CARTESIAN_POINT ( 'NONE',  ( 9.999999999999994671, -5.651611091574781476, -4.776954267060657955 ) ) ;
#10651 = ORIENTED_EDGE ( 'NONE', *, *, #9886, .F. ) ;
#10652 = CIRCLE ( 'NONE', #10856, 24.99999999999998934 ) ;
#10653 = ORIENTED_EDGE ( 'NONE', *, *, #4771, .T. ) ;
#10654 = CARTESIAN_POINT ( 'NONE',  ( 20.00000000000000000, 15.24625277455639072, -6.248133273622503481 ) ) ;
#10655 = EDGE_LOOP ( 'NONE', ( #4635, #9240, #178, #6949 ) ) ;
#10656 = DIRECTION ( 'NONE',  ( 1.000000000000000000, 1.081682119347366197E-16, -6.938893903907228378E-17 ) ) ;
#10657 = CARTESIAN_POINT ( 'NONE',  ( 19.99999999999999645, -2.720702104307051172, 5.902099716170436494 ) ) ;
#10658 = VERTEX_POINT ( 'NONE', #6711 ) ;
#10659 = EDGE_CURVE ( 'NONE', #10716, #479, #1221, .T. ) ;
#10660 = CARTESIAN_POINT ( 'NONE',  ( -17.00000000000002842, 19.99999999999998579, 9.850000000000047606 ) ) ;
#10661 = PLANE ( 'NONE',  #7906 ) ;
#10662 = AXIS2_PLACEMENT_3D ( 'NONE', #3525, #7758, #26 ) ;
#10663 = ORIENTED_EDGE ( 'NONE', *, *, #11790, .T. ) ;
#10664 = VERTEX_POINT ( 'NONE', #1742 ) ;
#10665 = AXIS2_PLACEMENT_3D ( 'NONE', #9821, #1017, #4110 ) ;
#10666 = ORIENTED_EDGE ( 'NONE', *, *, #6843, .T. ) ;
#10667 = CARTESIAN_POINT ( 'NONE',  ( 2.000000000000001776, 1.773042676681341856, -3.469446951953614189E-15 ) ) ;
#10668 = CIRCLE ( 'NONE', #8203, 2.149999999999985256 ) ;
#10669 = ORIENTED_EDGE ( 'NONE', *, *, #9501, .F. ) ;
#10670 = DIRECTION ( 'NONE',  ( 1.000000000000000000, 1.031065855027150586E-29, 2.218671295934092550E-30 ) ) ;
#10671 = ORIENTED_EDGE ( 'NONE', *, *, #5183, .F. ) ;
#10672 = EDGE_CURVE ( 'NONE', #9285, #6460, #9439, .T. ) ;
#10673 = CARTESIAN_POINT ( 'NONE',  ( 0.000000000000000000, -5.682309657208367781, 3.313524683561968942 ) ) ;
#10674 = ADVANCED_FACE ( 'NONE', ( #9455 ), #8501, .F. ) ;
#10675 = AXIS2_PLACEMENT_3D ( 'NONE', #12112, #10148, #7973 ) ;
#10676 = AXIS2_PLACEMENT_3D ( 'NONE', #5949, #988, #11886 ) ;
#10677 = CIRCLE ( 'NONE', #8833, 1.610000000000001874 ) ;
#10678 = DIRECTION ( 'NONE',  ( 1.000000000000000000, 0.000000000000000000, 0.000000000000000000 ) ) ;
#10679 = DIRECTION ( 'NONE',  ( -0.000000000000000000, -1.000000000000000000, -0.000000000000000000 ) ) ;
#10680 = EDGE_CURVE ( 'NONE', #12512, #2523, #4774, .T. ) ;
#10681 = ORIENTED_EDGE ( 'NONE', *, *, #978, .F. ) ;
#10682 = DIRECTION ( 'NONE',  ( 0.000000000000000000, 0.000000000000000000, 1.000000000000000000 ) ) ;
#10683 = ORIENTED_EDGE ( 'NONE', *, *, #6410, .T. ) ;
#10684 = DIRECTION ( 'NONE',  ( -1.000000000000000000, 0.000000000000000000, 0.000000000000000000 ) ) ;
#10685 = AXIS2_PLACEMENT_3D ( 'NONE', #6347, #10194, #3592 ) ;
#10687 = CIRCLE ( 'NONE', #5963, 1.000000000000000888 ) ;
#10686 = PRESENTATION_STYLE_ASSIGNMENT (( #6774 ) ) ;
#10688 = AXIS2_PLACEMENT_3D ( 'NONE', #1998, #6844, #10878 ) ;
#10689 = DIRECTION ( 'NONE',  ( -1.000000000000000000, 1.010728034814421376E-30, 1.090846720500930387E-30 ) ) ;
#10690 = CARTESIAN_POINT ( 'NONE',  ( 0.000000000000000000, -0.8732627748488687169, 7.348293143721422283 ) ) ;
#10691 = DIRECTION ( 'NONE',  ( 1.368180632492690774E-30, -0.8805955318567323387, -0.4738686624730094610 ) ) ;
#10692 = DIRECTION ( 'NONE',  ( -1.000000000000000000, 1.010728034814421376E-30, 1.090846720500930387E-30 ) ) ;
#10693 = CARTESIAN_POINT ( 'NONE',  ( 3.122502256758252770E-14, -4.862606272033112909, -3.745885042887444616 ) ) ;
#10694 = DIRECTION ( 'NONE',  ( 1.000000000000000000, -1.010728034814421376E-30, -1.090846720500930387E-30 ) ) ;
#10695 = MECHANICAL_DESIGN_GEOMETRIC_PRESENTATION_REPRESENTATION (  '', ( #3519 ), #11123 ) ;
#10696 = CARTESIAN_POINT ( 'NONE',  ( 19.99999999999997868, -1.623118704078857499, -6.293050665016890477 ) ) ;
#10697 = CARTESIAN_POINT ( 'NONE',  ( 40.00000000000000000, 39.34792583643766051, -19.21347054209566707 ) ) ;
#10698 = UNCERTAINTY_MEASURE_WITH_UNIT (LENGTH_MEASURE( 1.000000000000000082E-05 ), #9365, 'distance_accuracy_value', 'NONE');
#10699 = CARTESIAN_POINT ( 'NONE',  ( -4.000000000000012434, 1.539600717838998545, -3.300726591567094470 ) ) ;
#10700 = COLOUR_RGB ( '', 0.09019608, 0.27058824, 0.51372549) ;
#10701 = ORIENTED_EDGE ( 'NONE', *, *, #12123, .T. ) ;
#10702 = ORIENTED_EDGE ( 'NONE', *, *, #11676, .F. ) ;
#10703 = LINE ( 'NONE', #7044, #11804 ) ;
#10704 = FACE_OUTER_BOUND ( 'NONE', #4166, .T. ) ;
#10705 = DIRECTION ( 'NONE',  ( 0.000000000000000000, -1.224646799147353207E-16, 1.000000000000000000 ) ) ;
#10706 = FACE_OUTER_BOUND ( 'NONE', #4586, .T. ) ;
#10707 = ORIENTED_EDGE ( 'NONE', *, *, #12598, .F. ) ;
#10708 = CARTESIAN_POINT ( 'NONE',  ( 4.203833317240878387, 1.627343821129577872, -3.597273115243871722 ) ) ;
#10709 = LINE ( 'NONE', #218, #9128 ) ;
#10710 = AXIS2_PLACEMENT_3D ( 'NONE', #8201, #3394, #4540 ) ;
#10711 =( LENGTH_UNIT ( ) NAMED_UNIT ( * ) SI_UNIT ( .MILLI., .METRE. ) );
#10712 = ORIENTED_EDGE ( 'NONE', *, *, #3431, .F. ) ;
#10713 = ORIENTED_EDGE ( 'NONE', *, *, #11802, .F. ) ;
#10714 = EDGE_CURVE ( 'NONE', #7082, #8913, #12749, .T. ) ;
#10715 = CARTESIAN_POINT ( 'NONE',  ( 19.99999999999997868, 6.359534927042317598, 1.339147681075194996 ) ) ;
#10716 = VERTEX_POINT ( 'NONE', #2733 ) ;
#10717 = ORIENTED_EDGE ( 'NONE', *, *, #9401, .T. ) ;
#10718 = LINE ( 'NONE', #4752, #11716 ) ;
#10719 = ORIENTED_EDGE ( 'NONE', *, *, #3258, .T. ) ;
#10720 = CIRCLE ( 'NONE', #7647, 2.800000000000003819 ) ;
#10721 = DIRECTION ( 'NONE',  ( -3.260214209858707948E-30, -0.5000000000000012212, -0.8660254037844380415 ) ) ;
#10722 = CARTESIAN_POINT ( 'NONE',  ( 2.000000000000001776, 1.773042676681338303, 0.000000000000000000 ) ) ;
#10723 = VECTOR ( 'NONE', #7104, 1000.000000000000000 ) ;
#10724 = ORIENTED_EDGE ( 'NONE', *, *, #5884, .F. ) ;
#10725 = DIRECTION ( 'NONE',  ( -1.000000000000000000, 1.010728034814421376E-30, 1.090846720500930387E-30 ) ) ;
#10726 = CARTESIAN_POINT ( 'NONE',  ( 19.99999999999999645, -5.610543508060415796, -3.433640984893324699 ) ) ;
#10727 = ORIENTED_EDGE ( 'NONE', *, *, #8246, .F. ) ;
#10728 = EDGE_CURVE ( 'NONE', #8586, #962, #5981, .T. ) ;
#10729 = ORIENTED_EDGE ( 'NONE', *, *, #2520, .F. ) ;
#10730 = AXIS2_PLACEMENT_3D ( 'NONE', #11419, #903, #4837 ) ;
#10731 = EDGE_CURVE ( 'NONE', #12693, #5778, #6901, .T. ) ;
#10732 = ORIENTED_EDGE ( 'NONE', *, *, #4787, .T. ) ;
#10733 = DIRECTION ( 'NONE',  ( 1.000000000000000000, -6.162975822039154730E-33, -4.563833282352349791E-17 ) ) ;
#10734 = ORIENTED_EDGE ( 'NONE', *, *, #10167, .F. ) ;
#10735 = CARTESIAN_POINT ( 'NONE',  ( 2.171643655288379104, -3.365003104552334978, -1.177008749073000871E-14 ) ) ;
#10736 = EDGE_LOOP ( 'NONE', ( #7791, #475, #6305, #10316 ) ) ;
#10737 = CARTESIAN_POINT ( 'NONE',  ( 4.200000000000001954, 0.000000000000000000, -2.200000000000018385 ) ) ;
#10738 = VECTOR ( 'NONE', #464, 1000.000000000000000 ) ;
#10739 = CIRCLE ( 'NONE', #5203, 2.499999999999992006 ) ;
#10740 = DIRECTION ( 'NONE',  ( -1.000000000000000000, 1.010728034814421376E-30, 1.090846720500930387E-30 ) ) ;
#10741 = DIRECTION ( 'NONE',  ( -1.000000000000000000, 1.010728034814421376E-30, 1.090846720500930387E-30 ) ) ;
#10742 = ORIENTED_EDGE ( 'NONE', *, *, #4838, .F. ) ;
#10743 = DIRECTION ( 'NONE',  ( -1.000000000000000000, 0.000000000000000000, 0.000000000000000000 ) ) ;
#10744 = CIRCLE ( 'NONE', #10956, 1.535500000000000087 ) ;
#10745 = ORIENTED_EDGE ( 'NONE', *, *, #9565, .T. ) ;
#10746 = CYLINDRICAL_SURFACE ( 'NONE', #8052, 6.499000000000010324 ) ;
#10747 = CIRCLE ( 'NONE', #8495, 2.149999999999985256 ) ;
#10748 =( NAMED_UNIT ( * ) PLANE_ANGLE_UNIT ( ) SI_UNIT ( $, .RADIAN. ) );
#10749 = CARTESIAN_POINT ( 'NONE',  ( 27.00000000000001421, 39.34792583643766761, -17.06347054209568270 ) ) ;
#10750 = CARTESIAN_POINT ( 'NONE',  ( 19.99999999999999645, -6.413745496774076571, -3.691052519622334938 ) ) ;
#10751 = EDGE_CURVE ( 'NONE', #3763, #11641, #6589, .T. ) ;
#10752 = AXIS2_PLACEMENT_3D ( 'NONE', #7815, #12723, #3888 ) ;
#10753 = CARTESIAN_POINT ( 'NONE',  ( 33.00000000000001421, 39.34792583643766761, -17.06347054209568270 ) ) ;
#10754 = CARTESIAN_POINT ( 'NONE',  ( 1.747541505913291937, -3.837784562140264644, -3.503702292528917628 ) ) ;
#10755 = LINE ( 'NONE', #9657, #2578 ) ;
#10756 = CARTESIAN_POINT ( 'NONE',  ( 0.000000000000000000, 0.000000000000000000, 0.000000000000000000 ) ) ;
#10757 = FACE_OUTER_BOUND ( 'NONE', #8067, .T. ) ;
#10758 = ADVANCED_FACE ( 'NONE', ( #11857, #126 ), #8818, .F. ) ;
#10759 = DIRECTION ( 'NONE',  ( 1.000000000000000000, 1.849040895279789448E-31, -6.938893903907224680E-17 ) ) ;
#10760 = EDGE_CURVE ( 'NONE', #11435, #7272, #3048, .T. ) ;
#10761 = VECTOR ( 'NONE', #12456, 1000.000000000000000 ) ;
#10762 = APPLICATION_CONTEXT ( 'automotive_design' ) ;
#10763 = ORIENTED_EDGE ( 'NONE', *, *, #4895, .T. ) ;
#10764 = ORIENTED_EDGE ( 'NONE', *, *, #6176, .T. ) ;
#10765 = DIRECTION ( 'NONE',  ( 1.000000000000000000, -1.010728034814421376E-30, -1.090846720500930387E-30 ) ) ;
#10766 = CARTESIAN_POINT ( 'NONE',  ( 4.000000000000000000, -2.309401076758518911, -0.4999999999999917843 ) ) ;
#10767 = CYLINDRICAL_SURFACE ( 'NONE', #2662, 4.499999999999999112 ) ;
#10768 = PLANE ( 'NONE',  #11026 ) ;
#10769 = VERTEX_POINT ( 'NONE', #2059 ) ;
#10770 = VECTOR ( 'NONE', #2809, 1000.000000000000000 ) ;
#10771 = CARTESIAN_POINT ( 'NONE',  ( 4.211140560182196069, 2.431303136016537358, -3.745885042887416638 ) ) ;
#10772 = DIRECTION ( 'NONE',  ( 1.000000000000000000, -0.000000000000000000, -6.938893903907228378E-17 ) ) ;
#10773 = EDGE_CURVE ( 'NONE', #1427, #938, #3871, .T. ) ;
#10774 = SURFACE_STYLE_FILL_AREA ( #7052 ) ;
#10775 = ORIENTED_EDGE ( 'NONE', *, *, #9441, .F. ) ;
#10776 = ORIENTED_EDGE ( 'NONE', *, *, #3577, .T. ) ;
#10777 = CARTESIAN_POINT ( 'NONE',  ( 0.000000000000000000, 6.496448636052932990, -0.1820882179769771347 ) ) ;
#10778 = VERTEX_POINT ( 'NONE', #10810 ) ;
#10779 = AXIS2_PLACEMENT_3D ( 'NONE', #8770, #7683, #77 ) ;
#10780 = ORIENTED_EDGE ( 'NONE', *, *, #8084, .F. ) ;
#10781 = PRODUCT_CONTEXT ( 'NONE', #1732, 'mechanical' ) ;
#10782 = AXIS2_PLACEMENT_3D ( 'NONE', #2321, #3482, #5992 ) ;
#10783 = ADVANCED_FACE ( 'NONE', ( #1154 ), #1928, .T. ) ;
#10784 = DIRECTION ( 'NONE',  ( -1.000000000000000000, 0.000000000000000000, 0.000000000000000000 ) ) ;
#10785 = VERTEX_POINT ( 'NONE', #7975 ) ;
#10786 = CARTESIAN_POINT ( 'NONE',  ( 19.99999999999999645, 4.494880553659021061, 4.802513683199234329 ) ) ;
#10787 = EDGE_CURVE ( 'NONE', #7571, #10785, #6959, .T. ) ;
#10788 = CARTESIAN_POINT ( 'NONE',  ( -32.14999999999999147, 0.000000000000000000, 2.000000000000002220 ) ) ;
#10789 = ORIENTED_EDGE ( 'NONE', *, *, #360, .T. ) ;
#10790 = LINE ( 'NONE', #3028, #1597 ) ;
#10791 = FACE_OUTER_BOUND ( 'NONE', #7696, .T. ) ;
#10792 = AXIS2_PLACEMENT_3D ( 'NONE', #9639, #1924, #11791 ) ;
#10793 = EDGE_LOOP ( 'NONE', ( #10531, #1386, #5644, #10842 ) ) ;
#10794 = VERTEX_POINT ( 'NONE', #2128 ) ;
#10795 = VERTEX_POINT ( 'NONE', #5985 ) ;
#10796 = ADVANCED_FACE ( 'NONE', ( #9898 ), #6840, .T. ) ;
#10797 = FACE_OUTER_BOUND ( 'NONE', #7072, .T. ) ;
#10798 = B_SPLINE_CURVE_WITH_KNOTS ( 'NONE', 3,
 ( #5362, #720, #3507, #12519, #11360, #10441, #3695, #12264 ),
 .UNSPECIFIED., .F., .F.,
 ( 4, 2, 2, 4 ),
 ( 2.465131517098020131E-07, 0.001183067374689850647, 0.001774477805458922215, 0.002365888236227993349 ),
 .UNSPECIFIED. ) ;
#10799 = ORIENTED_EDGE ( 'NONE', *, *, #10234, .T. ) ;
#10800 = VECTOR ( 'NONE', #11884, 1000.000000000000000 ) ;
#10801 = DIRECTION ( 'NONE',  ( -1.000000000000000000, 1.010728034814421376E-30, 1.090846720500930387E-30 ) ) ;
#10802 = ORIENTED_EDGE ( 'NONE', *, *, #481, .F. ) ;
#10803 = EDGE_CURVE ( 'NONE', #10809, #5403, #3917, .T. ) ;
#10804 = ADVANCED_FACE ( 'NONE', ( #10940 ), #901, .T. ) ;
#10805 = EDGE_CURVE ( 'NONE', #4892, #6728, #2670, .T. ) ;
#10806 = FACE_OUTER_BOUND ( 'NONE', #442, .T. ) ;
#10807 = FACE_OUTER_BOUND ( 'NONE', #5008, .T. ) ;
#10808 = AXIS2_PLACEMENT_3D ( 'NONE', #11262, #1656, #1589 ) ;
#10809 = VERTEX_POINT ( 'NONE', #7793 ) ;
#10810 = CARTESIAN_POINT ( 'NONE',  ( 2.000000000000001776, -1.773042676681348739, 1.387778780781445676E-14 ) ) ;
#10811 = VERTEX_POINT ( 'NONE', #11729 ) ;
#10812 = FACE_OUTER_BOUND ( 'NONE', #6683, .T. ) ;
#10813 = CYLINDRICAL_SURFACE ( 'NONE', #7414, 2.800000000000003819 ) ;
#10814 = VECTOR ( 'NONE', #7504, 1000.000000000000114 ) ;
#10815 = CARTESIAN_POINT ( 'NONE',  ( 9.999999999999994671, 3.019282868015081611, 6.756029230465990132 ) ) ;
#10816 = AXIS2_PLACEMENT_3D ( 'NONE', #10897, #2083, #12602 ) ;
#10817 = CARTESIAN_POINT ( 'NONE',  ( 9.999999999999994671, 0.4528593230174703388, 7.386130139224206026 ) ) ;
#10818 = PRODUCT_DEFINITION ( 'UNKNOWN', '', #11667, #4881 ) ;
#10819 = LINE ( 'NONE', #1163, #9382 ) ;
#10820 = CARTESIAN_POINT ( 'NONE',  ( -3.999999999999991562, -1.942223658245627149, -0.3516579909967557649 ) ) ;
#10821 = LINE ( 'NONE', #12713, #11710 ) ;
#10822 = DIRECTION ( 'NONE',  ( -1.000000000000000000, 1.010728034814421376E-30, 1.090846720500930387E-30 ) ) ;
#10823 = EDGE_CURVE ( 'NONE', #12214, #1188, #2705, .T. ) ;
#10824 = AXIS2_PLACEMENT_3D ( 'NONE', #6071, #6325, #10232 ) ;
#10825 = FACE_OUTER_BOUND ( 'NONE', #1008, .T. ) ;
#10826 = ADVANCED_FACE ( 'NONE', ( #190 ), #1025, .T. ) ;
#10827 = ORIENTED_EDGE ( 'NONE', *, *, #4198, .T. ) ;
#10828 = CYLINDRICAL_SURFACE ( 'NONE', #11788, 2.800000000000003819 ) ;
#10829 = CARTESIAN_POINT ( 'NONE',  ( 11.00000000000003375, -6.123233995736744589E-16, 17.85000000000003695 ) ) ;
#10830 = AXIS2_PLACEMENT_3D ( 'NONE', #9510, #9445, #9571 ) ;
#10831 = CARTESIAN_POINT ( 'NONE',  ( 2.000000000000001776, 0.8865213383406622683, -1.535499999999995202 ) ) ;
#10832 = DIRECTION ( 'NONE',  ( -2.465190328815656418E-32, 1.177425296209236909E-30, 1.000000000000000000 ) ) ;
#10833 = CIRCLE ( 'NONE', #5498, 2.800000000000003375 ) ;
#10834 = EDGE_CURVE ( 'NONE', #11320, #10019, #4965, .T. ) ;
#10835 = LINE ( 'NONE', #11754, #8765 ) ;
#10836 = VERTEX_POINT ( 'NONE', #7911 ) ;
#10837 = VECTOR ( 'NONE', #12162, 1000.000000000000000 ) ;
#10838 = CARTESIAN_POINT ( 'NONE',  ( -45.00000000000012079, -19.99999999999999645, 2.000000000000007994 ) ) ;
#10839 = EDGE_CURVE ( 'NONE', #8571, #2734, #1653, .T. ) ;
#10840 = FACE_OUTER_BOUND ( 'NONE', #6735, .T. ) ;
#10841 = DIRECTION ( 'NONE',  ( 0.000000000000000000, -1.000000000000000000, 0.000000000000000000 ) ) ;
#10842 = ORIENTED_EDGE ( 'NONE', *, *, #8454, .T. ) ;
#10843 = ORIENTED_EDGE ( 'NONE', *, *, #5538, .F. ) ;
#10844 = EDGE_CURVE ( 'NONE', #9393, #303, #11538, .T. ) ;
#10845 = FACE_OUTER_BOUND ( 'NONE', #10183, .T. ) ;
#10846 = ORIENTED_EDGE ( 'NONE', *, *, #6897, .T. ) ;
#10847 = ORIENTED_EDGE ( 'NONE', *, *, #4435, .T. ) ;
#10848 = APPLICATION_PROTOCOL_DEFINITION ( 'draft international standard', 'automotive_design', 1998, #10762 ) ;
#10849 = CARTESIAN_POINT ( 'NONE',  ( 20.00000000000000000, 5.510332127717284397E-15, -2.499999999999999556 ) ) ;
#10850 = VERTEX_POINT ( 'NONE', #10091 ) ;
#10851 = CARTESIAN_POINT ( 'NONE',  ( 19.99999999999997868, -0.8732627748487620245, -7.348293143721449816 ) ) ;
#10852 = CARTESIAN_POINT ( 'NONE',  ( 15.00000000000003375, 30.00000000000001776, -9.742497179615118866E-31 ) ) ;
#10853 = VERTEX_POINT ( 'NONE', #3304 ) ;
#10854 = FACE_OUTER_BOUND ( 'NONE', #2009, .T. ) ;
#10855 = DIRECTION ( 'NONE',  ( 1.000000000000000000, 1.849040895279789448E-31, -6.938893903907224680E-17 ) ) ;
#10856 = AXIS2_PLACEMENT_3D ( 'NONE', #7597, #6764, #7788 ) ;
#10857 = ORIENTED_EDGE ( 'NONE', *, *, #10644, .T. ) ;
#10858 = ORIENTED_EDGE ( 'NONE', *, *, #2018, .F. ) ;
#10859 = ORIENTED_EDGE ( 'NONE', *, *, #6410, .F. ) ;
#10860 = CARTESIAN_POINT ( 'NONE',  ( 0.000000000000000000, -1.966014849756989147, -6.277170897746302991 ) ) ;
#10861 = CARTESIAN_POINT ( 'NONE',  ( 0.02511973781851166085, -4.877415612947438639, -3.751298745799855894 ) ) ;
#10862 = VERTEX_POINT ( 'NONE', #5216 ) ;
#10863 = DIRECTION ( 'NONE',  ( -2.312964634635743450E-16, 0.9883022714608525883, -0.1525077710325583313 ) ) ;
#10864 = AXIS2_PLACEMENT_3D ( 'NONE', #6732, #2945, #3890 ) ;
#10865 = EDGE_LOOP ( 'NONE', ( #12544, #12612, #10407, #9276 ) ) ;
#10866 = DIRECTION ( 'NONE',  ( 0.000000000000000000, 0.000000000000000000, 1.000000000000000000 ) ) ;
#10867 = AXIS2_PLACEMENT_3D ( 'NONE', #9070, #251, #8103 ) ;
#10868 = AXIS2_PLACEMENT_3D ( 'NONE', #244, #4175, #8096 ) ;
#10869 = DIRECTION ( 'NONE',  ( 1.000000000000000000, 5.916456789157576279E-31, 0.000000000000000000 ) ) ;
#10870 = ORIENTED_EDGE ( 'NONE', *, *, #5441, .T. ) ;
#10871 = AXIS2_PLACEMENT_3D ( 'NONE', #10786, #5770, #9875 ) ;
#10872 = DIRECTION ( 'NONE',  ( 1.000000000000000000, -1.010728034814421376E-30, -1.090846720500930387E-30 ) ) ;
#10873 = EDGE_LOOP ( 'NONE', ( #10998, #999, #6353, #4022 ) ) ;
#10874 = DIRECTION ( 'NONE',  ( -1.000000000000000000, 1.010728034814421376E-30, 1.090846720500930387E-30 ) ) ;
#10875 = EDGE_CURVE ( 'NONE', #4176, #1508, #11113, .T. ) ;
#10876 = EDGE_CURVE ( 'NONE', #9949, #12174, #3176, .T. ) ;
#10877 = SURFACE_STYLE_USAGE ( .BOTH. , #6053 ) ;
#10878 = DIRECTION ( 'NONE',  ( 0.000000000000000000, 0.7818314824680310249, -0.6234898018587319291 ) ) ;
#10879 = CIRCLE ( 'NONE', #1628, 2.800000000000003819 ) ;
#10880 = VECTOR ( 'NONE', #850, 1000.000000000000000 ) ;
#10881 = CIRCLE ( 'NONE', #7810, 6.499000000000009436 ) ;
#10882 = DIRECTION ( 'NONE',  ( -1.000000000000000000, 1.010728034814421376E-30, 1.090846720500930387E-30 ) ) ;
#10883 = DIRECTION ( 'NONE',  ( 0.000000000000000000, 0.000000000000000000, 1.000000000000000000 ) ) ;
#10884 = CARTESIAN_POINT ( 'NONE',  ( 4.000000000000003553, 0.000000000000000000, 0.000000000000000000 ) ) ;
#10885 = CARTESIAN_POINT ( 'NONE',  ( 11.00000000000003020, 30.00000000000000000, 4.999999999999999112 ) ) ;
#10886 = DIRECTION ( 'NONE',  ( 0.000000000000000000, -0.08963930890344097568, 0.9959742939952382912 ) ) ;
#10887 = DIRECTION ( 'NONE',  ( 0.000000000000000000, 0.000000000000000000, 1.000000000000000000 ) ) ;
#10888 = VECTOR ( 'NONE', #9517, 1000.000000000000000 ) ;
#10889 = AXIS2_PLACEMENT_3D ( 'NONE', #12318, #3378, #7295 ) ;
#10890 = AXIS2_PLACEMENT_3D ( 'NONE', #7227, #2331, #2394 ) ;
#10891 = CARTESIAN_POINT ( 'NONE',  ( 19.99999999999997868, 0.2252065540230664964, -6.573992004634869879 ) ) ;
#10892 = EDGE_CURVE ( 'NONE', #10836, #3366, #11385, .T. ) ;
#10893 = ORIENTED_EDGE ( 'NONE', *, *, #3587, .T. ) ;
#10894 = ORIENTED_EDGE ( 'NONE', *, *, #2278, .T. ) ;
#10895 = DIRECTION ( 'NONE',  ( -1.000000000000000000, 1.006188713385347367E-17, 3.844790828812615713E-17 ) ) ;
#10896 = AXIS2_PLACEMENT_3D ( 'NONE', #10588, #677, #4615 ) ;
#10897 = CARTESIAN_POINT ( 'NONE',  ( 19.99999999999999645, 0.000000000000000000, 0.000000000000000000 ) ) ;
#10898 = DIRECTION ( 'NONE',  ( 0.000000000000000000, 1.000000000000000000, 1.224646799147353207E-16 ) ) ;
#10899 = VECTOR ( 'NONE', #1399, 1000.000000000000000 ) ;
#10900 = DIRECTION ( 'NONE',  ( 0.000000000000000000, 0.000000000000000000, 1.000000000000000000 ) ) ;
#10901 = VERTEX_POINT ( 'NONE', #2260 ) ;
#10902 = DIRECTION ( 'NONE',  ( 0.000000000000000000, -0.4999999999999992784, 0.8660254037844389297 ) ) ;
#10903 = DIRECTION ( 'NONE',  ( -1.031065855027149465E-29, -1.000000000000000000, 7.771561172376086908E-16 ) ) ;
#10904 = CARTESIAN_POINT ( 'NONE',  ( 9.000000000000031974, 12.50000000000000000, 5.000000000000004441 ) ) ;
#10905 = VERTEX_POINT ( 'NONE', #5581 ) ;
#10906 = ORIENTED_EDGE ( 'NONE', *, *, #10165, .T. ) ;
#10907 = CARTESIAN_POINT ( 'NONE',  ( 0.000000000000000000, -4.999339924971534899, -4.274890546384045642 ) ) ;
#10908 = ORIENTED_EDGE ( 'NONE', *, *, #2270, .F. ) ;
#10909 = VERTEX_POINT ( 'NONE', #2327 ) ;
#10910 = APPLICATION_PROTOCOL_DEFINITION ( 'draft international standard', 'automotive_design', 1998, #12106 ) ;
#10911 = ADVANCED_FACE ( 'NONE', ( #9133 ), #11010, .T. ) ;
#10912 = ADVANCED_FACE ( 'NONE', ( #9361, #6491, #12115, #2196 ), #619, .F. ) ;
#10913 = CARTESIAN_POINT ( 'NONE',  ( -18.00000000000002842, -30.00000000000000000, 2.000000000000004441 ) ) ;
#10914 = ORIENTED_EDGE ( 'NONE', *, *, #11963, .T. ) ;
#10915 = SURFACE_STYLE_FILL_AREA ( #43 ) ;
#10916 = CARTESIAN_POINT ( 'NONE',  ( 19.99999999999999645, 0.000000000000000000, 0.000000000000000000 ) ) ;
#10917 = ORIENTED_EDGE ( 'NONE', *, *, #5219, .F. ) ;
#10918 = FACE_OUTER_BOUND ( 'NONE', #3474, .T. ) ;
#10919 = EDGE_CURVE ( 'NONE', #1807, #6277, #7156, .T. ) ;
#10920 = DIRECTION ( 'NONE',  ( 1.000000000000000000, 0.000000000000000000, -2.168404344971007882E-16 ) ) ;
#10921 = AXIS2_PLACEMENT_3D ( 'NONE', #12150, #1439, #9219 ) ;
#10922 = EDGE_LOOP ( 'NONE', ( #3960, #8929, #2326, #3341 ) ) ;
#10923 = VERTEX_POINT ( 'NONE', #8176 ) ;
#10924 = ORIENTED_EDGE ( 'NONE', *, *, #6204, .F. ) ;
#10925 = VECTOR ( 'NONE', #5675, 1000.000000000000000 ) ;
#10926 = CARTESIAN_POINT ( 'NONE',  ( 19.99999999999999645, 0.6915992404089836842, 6.462096524400245734 ) ) ;
#10927 = ADVANCED_FACE ( 'NONE', ( #10398 ), #7222, .F. ) ;
#10928 = AXIS2_PLACEMENT_3D ( 'NONE', #4915, #8834, #12063 ) ;
#10929 = CARTESIAN_POINT ( 'NONE',  ( -1.274258131565009000, -3.883108878240904449, -3.220599429843879147 ) ) ;
#10930 = ORIENTED_EDGE ( 'NONE', *, *, #12582, .T. ) ;
#10931 = CARTESIAN_POINT ( 'NONE',  ( 0.000000000000000000, 30.00000000000000000, 0.000000000000000000 ) ) ;
#10932 = ORIENTED_EDGE ( 'NONE', *, *, #304, .T. ) ;
#10933 = CARTESIAN_POINT ( 'NONE',  ( 14.00000000000000000, 12.99999999999999822, 0.000000000000000000 ) ) ;
#10934 = DIRECTION ( 'NONE',  ( 0.000000000000000000, -0.5877852522924802425, 0.8090169943749422332 ) ) ;
#10935 = AXIS2_PLACEMENT_3D ( 'NONE', #7542, #4776, #12389 ) ;
#10936 = PRODUCT_DEFINITION_CONTEXT ( 'detailed design', #4366, 'design' ) ;
#10937 = DIRECTION ( 'NONE',  ( 0.000000000000000000, 0.000000000000000000, 1.000000000000000000 ) ) ;
#10938 =( REPRESENTATION_RELATIONSHIP ('NONE','NONE', #10018, #9199 ) REPRESENTATION_RELATIONSHIP_WITH_TRANSFORMATION ( #1312 )SHAPE_REPRESENTATION_RELATIONSHIP( ) );
#10939 = ORIENTED_EDGE ( 'NONE', *, *, #10039, .F. ) ;
#10940 = FACE_OUTER_BOUND ( 'NONE', #4111, .T. ) ;
#10941 = EDGE_LOOP ( 'NONE', ( #10924, #12308, #1887, #5980 ) ) ;
#10942 = CARTESIAN_POINT ( 'NONE',  ( 12.94787914004603557, 12.50000000000000000, 5.638155724715463002 ) ) ;
#10943 = ADVANCED_FACE ( 'NONE', ( #12420 ), #3595, .T. ) ;
#10944 = CARTESIAN_POINT ( 'NONE',  ( 14.00000000000000000, -30.00000000000000000, 0.000000000000000000 ) ) ;
#10945 = AXIS2_PLACEMENT_3D ( 'NONE', #12185, #5343, #7347 ) ;
#10946 = DIRECTION ( 'NONE',  ( -1.000000000000000000, 0.000000000000000000, 0.000000000000000000 ) ) ;
#10947 = ADVANCED_BREP_SHAPE_REPRESENTATION ( '', ( #1664, #12422 ), #10082 ) ;
#10948 = DIRECTION ( 'NONE',  ( 0.000000000000000000, 1.000000000000000000, 0.000000000000000000 ) ) ;
#10949 = DIRECTION ( 'NONE',  ( 0.000000000000000000, 4.478906847412178337E-32, -1.000000000000000000 ) ) ;
#10950 = DIRECTION ( 'NONE',  ( -1.000000000000000000, -5.916456789157575403E-31, 1.577021341797098793E-16 ) ) ;
#10951 = AXIS2_PLACEMENT_3D ( 'NONE', #8836, #22, #7872 ) ;
#10952 = CIRCLE ( 'NONE', #11789, 6.999999999999999112 ) ;
#10953 = DIRECTION ( 'NONE',  ( -1.000000000000000000, 0.000000000000000000, 0.000000000000000000 ) ) ;
#10954 = CARTESIAN_POINT ( 'NONE',  ( 11.00000000000001599, 19.99999999999999645, 12.00000000000003020 ) ) ;
#10955 =( LENGTH_UNIT ( ) NAMED_UNIT ( * ) SI_UNIT ( .MILLI., .METRE. ) );
#10956 = AXIS2_PLACEMENT_3D ( 'NONE', #10001, #11897, #9877 ) ;
#10957 = ORIENTED_EDGE ( 'NONE', *, *, #254, .T. ) ;
#10958 = DIRECTION ( 'NONE',  ( -1.000000000000000000, 1.010728034814421376E-30, 1.090846720500930387E-30 ) ) ;
#10959 = DIRECTION ( 'NONE',  ( -1.000000000000000000, 1.010728034814421376E-30, 1.090846720500930387E-30 ) ) ;
#10960 = CARTESIAN_POINT ( 'NONE',  ( -3.999999999999993339, 2.511478553582019213, -3.469254451724774757 ) ) ;
#10961 = PLANE ( 'NONE',  #1821 ) ;
#10962 = DIRECTION ( 'NONE',  ( -1.000000000000000000, 1.010728034814421376E-30, 1.090846720500930387E-30 ) ) ;
#10963 = ORIENTED_EDGE ( 'NONE', *, *, #10165, .F. ) ;
#10964 = EDGE_CURVE ( 'NONE', #2228, #6027, #10464, .T. ) ;
#10965 = CARTESIAN_POINT ( 'NONE',  ( 0.000000000000000000, -30.00000000000000000, 0.000000000000000000 ) ) ;
#10966 = EDGE_CURVE ( 'NONE', #11848, #4250, #681, .T. ) ;
#10967 = EDGE_CURVE ( 'NONE', #5083, #11532, #9859, .T. ) ;
#10968 = DIRECTION ( 'NONE',  ( 1.140150527077241873E-30, 0.000000000000000000, -1.000000000000000000 ) ) ;
#10969 = EDGE_CURVE ( 'NONE', #3923, #7484, #10024, .T. ) ;
#10970 = LINE ( 'NONE', #6141, #5140 ) ;
#10971 = VECTOR ( 'NONE', #6795, 1000.000000000000000 ) ;
#10972 = ORIENTED_EDGE ( 'NONE', *, *, #4861, .T. ) ;
#10973 = CYLINDRICAL_SURFACE ( 'NONE', #6629, 2.500000000000000444 ) ;
#10974 = ORIENTED_EDGE ( 'NONE', *, *, #445, .F. ) ;
#10975 = ORIENTED_EDGE ( 'NONE', *, *, #12095, .T. ) ;
#10976 = PRODUCT_CONTEXT ( 'NONE', #409, 'mechanical' ) ;
#10977 = EDGE_CURVE ( 'NONE', #11940, #11433, #3689, .T. ) ;
#10978 = LINE ( 'NONE', #2165, #5965 ) ;
#10979 = ORIENTED_EDGE ( 'NONE', *, *, #2077, .F. ) ;
#10980 = AXIS2_PLACEMENT_3D ( 'NONE', #279, #12146, #471 ) ;
#10981 = SURFACE_STYLE_FILL_AREA ( #480 ) ;
#10982 = DIRECTION ( 'NONE',  ( -1.000000000000000000, 1.010728034814421376E-30, 1.090846720500930387E-30 ) ) ;
#10983 = ORIENTED_EDGE ( 'NONE', *, *, #11688, .T. ) ;
#10984 = AXIS2_PLACEMENT_3D ( 'NONE', #2512, #6501, #12370 ) ;
#10985 = FILL_AREA_STYLE_COLOUR ( '', #6095 ) ;
#10986 = DIRECTION ( 'NONE',  ( 0.000000000000000000, -1.000000000000000000, 0.000000000000000000 ) ) ;
#10987 = LINE ( 'NONE', #1385, #12506 ) ;
#10988 = LINE ( 'NONE', #8925, #1948 ) ;
#10989 = EDGE_CURVE ( 'NONE', #10862, #9583, #6179, .T. ) ;
#10990 = ORIENTED_EDGE ( 'NONE', *, *, #111, .T. ) ;
#10991 = AXIS2_PLACEMENT_3D ( 'NONE', #3557, #1738, #12253 ) ;
#10992 = ORIENTED_EDGE ( 'NONE', *, *, #8152, .F. ) ;
#10993 = VERTEX_POINT ( 'NONE', #11635 ) ;
#10994 = VERTEX_POINT ( 'NONE', #1713 ) ;
#10995 = CARTESIAN_POINT ( 'NONE',  ( 19.99999999999997868, 2.918117354836732513, -5.807029542149833468 ) ) ;
#10996 = EDGE_CURVE ( 'NONE', #11547, #3660, #11512, .T. ) ;
#10997 = DIRECTION ( 'NONE',  ( 1.000000000000000000, 1.081682119347366197E-16, -6.938893903907228378E-17 ) ) ;
#10998 = ORIENTED_EDGE ( 'NONE', *, *, #12288, .T. ) ;
#10999 = EDGE_CURVE ( 'NONE', #9579, #8089, #623, .T. ) ;
#11000 = CARTESIAN_POINT ( 'NONE',  ( 4.000000000000000000, 0.000000000000000000, 0.000000000000000000 ) ) ;
#11001 = EDGE_LOOP ( 'NONE', ( #940, #5259, #3596, #7721 ) ) ;
#11002 = CIRCLE ( 'NONE', #12655, 7.400000000000009237 ) ;
#11003 = CIRCLE ( 'NONE', #6276, 0.2000000000000000944 ) ;
#11004 = CARTESIAN_POINT ( 'NONE',  ( -2.855764796983343956, 2.970025579236416746, -0.09382832055445594621 ) ) ;
#11005 = ADVANCED_FACE ( 'NONE', ( #2830 ), #867, .T. ) ;
#11006 = EDGE_CURVE ( 'NONE', #12032, #6829, #3086, .T. ) ;
#11007 = CARTESIAN_POINT ( 'NONE',  ( 19.99999999999999645, -5.932103089875909951, -2.654647609586772816 ) ) ;
#11008 = LINE ( 'NONE', #5214, #8223 ) ;
#11009 = ORIENTED_EDGE ( 'NONE', *, *, #1314, .F. ) ;
#11010 = CYLINDRICAL_SURFACE ( 'NONE', #4296, 2.800000000000003819 ) ;
#11011 = AXIS2_PLACEMENT_3D ( 'NONE', #9987, #6929, #10968 ) ;
#11012 = ORIENTED_EDGE ( 'NONE', *, *, #9960, .T. ) ;
#11013 = CONICAL_SURFACE ( 'NONE', #6488, 2.059999999999998721, 0.9599310885968738161 ) ;
#11014 = DIRECTION ( 'NONE',  ( -1.000000000000000000, 0.000000000000000000, 0.000000000000000000 ) ) ;
#11015 = SURFACE_STYLE_FILL_AREA ( #7094 ) ;
#11016 = DIRECTION ( 'NONE',  ( -1.000000000000000000, -1.031065855027150586E-29, 2.218671295934095703E-30 ) ) ;
#11017 = CYLINDRICAL_SURFACE ( 'NONE', #7030, 4.000000000000000000 ) ;
#11018 = LINE ( 'NONE', #135, #8782 ) ;
#11019 = AXIS2_PLACEMENT_3D ( 'NONE', #10376, #722, #2745 ) ;
#11020 = B_SPLINE_CURVE_WITH_KNOTS ( 'NONE', 3,
 ( #11661, #5662, #12573, #7667 ),
 .UNSPECIFIED., .F., .F.,
 ( 4, 4 ),
 ( 0.000000000000000000, 0.002452478801916380645 ),
 .UNSPECIFIED. ) ;
#11021 = DIRECTION ( 'NONE',  ( 0.000000000000000000, -1.000000000000000000, 0.000000000000000000 ) ) ;
#11022 = CARTESIAN_POINT ( 'NONE',  ( 19.99999999999997868, 2.180689217871956131, -6.122221454264557217 ) ) ;
#11023 = DIRECTION ( 'NONE',  ( -1.000000000000000000, -5.916456789157575403E-31, -2.465190328815656418E-32 ) ) ;
#11024 = CYLINDRICAL_SURFACE ( 'NONE', #4770, 2.149999999999988809 ) ;
#11025 = ADVANCED_FACE ( 'NONE', ( #8668, #3656 ), #12611, .F. ) ;
#11026 = AXIS2_PLACEMENT_3D ( 'NONE', #5696, #7759, #9794 ) ;
#11027 = AXIS2_PLACEMENT_3D ( 'NONE', #242, #11064, #1076 ) ;
#11028 = ORIENTED_EDGE ( 'NONE', *, *, #8545, .F. ) ;
#11029 = DIRECTION ( 'NONE',  ( -1.000000000000000000, 1.010728034814421376E-30, 1.090846720500930387E-30 ) ) ;
#11030 = DIRECTION ( 'NONE',  ( -0.000000000000000000, -1.000000000000000000, -0.000000000000000000 ) ) ;
#11031 = CARTESIAN_POINT ( 'NONE',  ( -4.203934362469355257, -1.640673743454835520, -3.598432614607002034 ) ) ;
#11032 = DIRECTION ( 'NONE',  ( 1.232595164407829369E-30, -0.9510565162951500895, -0.3090169943749582759 ) ) ;
#11033 = VERTEX_POINT ( 'NONE', #2955 ) ;
#11034 = CARTESIAN_POINT ( 'NONE',  ( 0.000000000000000000, 5.200656487704269360, 5.264330166022977764 ) ) ;
#11035 = AXIS2_PLACEMENT_3D ( 'NONE', #11490, #9466, #5496 ) ;
#11036 = DIRECTION ( 'NONE',  ( 0.000000000000000000, 1.000000000000000000, 0.000000000000000000 ) ) ;
#11037 = AXIS2_PLACEMENT_3D ( 'NONE', #9410, #3646, #8400 ) ;
#11038 = DIRECTION ( 'NONE',  ( 1.848892746611746419E-31, 1.000000000000000000, -3.250006781153460502E-32 ) ) ;
#11039 = ORIENTED_EDGE ( 'NONE', *, *, #758, .F. ) ;
#11040 = DIRECTION ( 'NONE',  ( -1.000000000000000000, 1.010728034814421376E-30, 1.090846720500930387E-30 ) ) ;
#11041 = ORIENTED_EDGE ( 'NONE', *, *, #11725, .T. ) ;
#11042 = VERTEX_POINT ( 'NONE', #805 ) ;
#11043 = APPLICATION_PROTOCOL_DEFINITION ( 'draft international standard', 'automotive_design', 1998, #2 ) ;
#11044 = ADVANCED_FACE ( 'NONE', ( #9552 ), #7572, .T. ) ;
#11045 = ORIENTED_EDGE ( 'NONE', *, *, #7462, .T. ) ;
#11046 = DIRECTION ( 'NONE',  ( -1.000000000000000000, 1.010728034814421376E-30, 1.090846720500930387E-30 ) ) ;
#11047 = ADVANCED_FACE ( 'NONE', ( #1835 ), #10530, .T. ) ;
#11048 = ORIENTED_EDGE ( 'NONE', *, *, #11688, .F. ) ;
#11049 = AXIS2_PLACEMENT_3D ( 'NONE', #4657, #3757, #7682 ) ;
#11050 = LINE ( 'NONE', #12218, #7792 ) ;
#11051 = VECTOR ( 'NONE', #12330, 1000.000000000000000 ) ;
#11052 = DIRECTION ( 'NONE',  ( 0.000000000000000000, 0.000000000000000000, 1.000000000000000000 ) ) ;
#11053 = EDGE_LOOP ( 'NONE', ( #5781, #4866, #4217, #9329 ) ) ;
#11054 = CARTESIAN_POINT ( 'NONE',  ( 40.00000000000000711, 19.99999999999999645, -9.850000000000013856 ) ) ;
#11055 = CARTESIAN_POINT ( 'NONE',  ( 0.000000000000000000, 0.000000000000000000, 0.000000000000000000 ) ) ;
#11056 = CYLINDRICAL_SURFACE ( 'NONE', #7359, 2.149999999999988809 ) ;
#11057 = CARTESIAN_POINT ( 'NONE',  ( -3.436319922987216557, 2.634841920960315775, -3.531542292955241358 ) ) ;
#11058 = VERTEX_POINT ( 'NONE', #10777 ) ;
#11059 = ORIENTED_EDGE ( 'NONE', *, *, #12265, .F. ) ;
#11060 = CIRCLE ( 'NONE', #768, 9.999999999999998224 ) ;
#11061 = EDGE_LOOP ( 'NONE', ( #82, #9823, #3705, #1073 ) ) ;
#11062 = VERTEX_POINT ( 'NONE', #7641 ) ;
#11063 = CARTESIAN_POINT ( 'NONE',  ( 2.100000000000000089, 0.000000000000000000, -0.2800830152838839626 ) ) ;
#11064 = DIRECTION ( 'NONE',  ( -1.000000000000000000, 1.010728034814421376E-30, 1.090846720500930387E-30 ) ) ;
#11065 = VERTEX_POINT ( 'NONE', #11577 ) ;
#11066 = CYLINDRICAL_SURFACE ( 'NONE', #4513, 9.999999999999998224 ) ;
#11067 = VERTEX_POINT ( 'NONE', #12674 ) ;
#11068 = DIRECTION ( 'NONE',  ( 0.000000000000000000, 0.000000000000000000, 1.000000000000000000 ) ) ;
#11069 = DIRECTION ( 'NONE',  ( 0.000000000000000000, 0.000000000000000000, -1.000000000000000000 ) ) ;
#11070 = PRODUCT_DEFINITION_CONTEXT ( 'detailed design', #2906, 'design' ) ;
#11071 = CARTESIAN_POINT ( 'NONE',  ( 0.000000000000000000, -7.258495115966587363, 1.440225208600799611 ) ) ;
#11072 = ORIENTED_EDGE ( 'NONE', *, *, #9651, .T. ) ;
#11073 = CARTESIAN_POINT ( 'NONE',  ( 27.00000000000001421, 39.34792583643766761, -17.06347054209568270 ) ) ;
#11074 = VERTEX_POINT ( 'NONE', #2702 ) ;
#11075 = CARTESIAN_POINT ( 'NONE',  ( 19.99999999999997868, 6.557268578288196537, 3.319920822022206952 ) ) ;
#11076 = CIRCLE ( 'NONE', #1196, 2.800000000000003819 ) ;
#11077 = EDGE_CURVE ( 'NONE', #12092, #3334, #1962, .T. ) ;
#11078 = CARTESIAN_POINT ( 'NONE',  ( 19.99999999999997868, 3.908107171477257058, -5.192658214849914522 ) ) ;
#11079 = ADVANCED_FACE ( 'NONE', ( #6871 ), #9802, .T. ) ;
#11080 = CYLINDRICAL_SURFACE ( 'NONE', #264, 2.149999999999988809 ) ;
#11081 = VECTOR ( 'NONE', #6553, 1000.000000000000114 ) ;
#11082 = CARTESIAN_POINT ( 'NONE',  ( -3.679171394226032454, -2.494631558665832305, -0.3503314178412488822 ) ) ;
#11083 = EDGE_CURVE ( 'NONE', #3794, #5369, #8537, .T. ) ;
#11084 = DIRECTION ( 'NONE',  ( 1.848892746611746419E-31, 1.000000000000000000, 3.250006781153453386E-32 ) ) ;
#11085 = AXIS2_PLACEMENT_3D ( 'NONE', #8738, #9683, #4028 ) ;
#11086 = FACE_OUTER_BOUND ( 'NONE', #6809, .T. ) ;
#11087 = DIRECTION ( 'NONE',  ( -1.000000000000000000, 1.010728034814421376E-30, 1.090846720500930387E-30 ) ) ;
#11088 = CARTESIAN_POINT ( 'NONE',  ( 40.00000000000000711, 10.63631887905126128, -9.927230231572499619 ) ) ;
#11089 = CIRCLE ( 'NONE', #11517, 2.499999999999992006 ) ;
#11090 = CIRCLE ( 'NONE', #8616, 7.400000000000009237 ) ;
#11092 = VECTOR ( 'NONE', #10378, 1000.000000000000114 ) ;
#11091 = PRESENTATION_STYLE_ASSIGNMENT (( #6812 ) ) ;
#11093 = AXIS2_PLACEMENT_3D ( 'NONE', #12548, #3845, #2773 ) ;
#11094 = ORIENTED_EDGE ( 'NONE', *, *, #6846, .T. ) ;
#11095 = CARTESIAN_POINT ( 'NONE',  ( 40.00000000000000711, 21.12780530657007816, -5.807015647486885257 ) ) ;
#11096 = LINE ( 'NONE', #12070, #5827 ) ;
#11097 = CARTESIAN_POINT ( 'NONE',  ( -3.999999999999993339, 0.8576368993457464951, -3.433240632782212032 ) ) ;
#11098 = FACE_OUTER_BOUND ( 'NONE', #3550, .T. ) ;
#11099 = ORIENTED_EDGE ( 'NONE', *, *, #3001, .F. ) ;
#11100 = CYLINDRICAL_SURFACE ( 'NONE', #5474, 6.999999999999999112 ) ;
#11101 = AXIS2_PLACEMENT_3D ( 'NONE', #9453, #8438, #7603 ) ;
#11102 = AXIS2_PLACEMENT_3D ( 'NONE', #10622, #12448, #836 ) ;
#11103 = CYLINDRICAL_SURFACE ( 'NONE', #1112, 10.00000000000000178 ) ;
#11104 = PRODUCT_DEFINITION_SHAPE ( 'NONE', 'NONE',  #4376 ) ;
#11105 = LINE ( 'NONE', #4273, #8215 ) ;
#11106 = ORIENTED_EDGE ( 'NONE', *, *, #9881, .T. ) ;
#11107 = DIRECTION ( 'NONE',  ( -1.000000000000000000, 1.010728034814421376E-30, 1.090846720500930387E-30 ) ) ;
#11108 = ORIENTED_EDGE ( 'NONE', *, *, #4840, .T. ) ;
#11109 = ORIENTED_EDGE ( 'NONE', *, *, #8325, .T. ) ;
#11110 = ITEM_DEFINED_TRANSFORMATION ( 'NONE', 'NONE', #4668,  #12422 ) ;
#11111 =( GEOMETRIC_REPRESENTATION_CONTEXT ( 3 ) GLOBAL_UNCERTAINTY_ASSIGNED_CONTEXT ( ( #786 ) ) GLOBAL_UNIT_ASSIGNED_CONTEXT ( ( #10711, #6618, #9548 ) ) REPRESENTATION_CONTEXT ( 'NONE', 'WORKASPACE' ) );
#11112 = CARTESIAN_POINT ( 'NONE',  ( 15.00000000000003375, 30.00000000000001776, -9.742497179615118866E-31 ) ) ;
#11113 = CIRCLE ( 'NONE', #6598, 6.000000000000000000 ) ;
#11114 = VERTEX_POINT ( 'NONE', #10593 ) ;
#11115 = CIRCLE ( 'NONE', #9044, 6.999999999999999112 ) ;
#11116 = CARTESIAN_POINT ( 'NONE',  ( 19.99999999999997868, 2.520781513113738548, -6.075668640744172677 ) ) ;
#11117 = DIRECTION ( 'NONE',  ( -1.000000000000000000, 1.010728034814421376E-30, 1.090846720500930387E-30 ) ) ;
#11118 = DIRECTION ( 'NONE',  ( -1.000000000000000000, -1.081682119347366197E-16, 6.938893903907228378E-17 ) ) ;
#11119 = DIRECTION ( 'NONE',  ( -1.000000000000000000, 1.010728034814421376E-30, 1.090846720500930387E-30 ) ) ;
#11120 = CARTESIAN_POINT ( 'NONE',  ( -1.360585162435275164, 4.061296242128064726, -3.505054077164865500 ) ) ;
#11121 = ADVANCED_BREP_SHAPE_REPRESENTATION ( '', ( #5784, #12422 ), #6859 ) ;
#11122 = ADVANCED_FACE ( 'NONE', ( #4677 ), #5763, .F. ) ;
#11123 =( GEOMETRIC_REPRESENTATION_CONTEXT ( 3 ) GLOBAL_UNCERTAINTY_ASSIGNED_CONTEXT ( ( #4788 ) ) GLOBAL_UNIT_ASSIGNED_CONTEXT ( ( #10955, #2143, #9679 ) ) REPRESENTATION_CONTEXT ( 'NONE', 'WORKASPACE' ) );
#11124 = EDGE_LOOP ( 'NONE', ( #2122, #5710, #3226 ) ) ;
#11125 = ORIENTED_EDGE ( 'NONE', *, *, #7752, .F. ) ;
#11126 = EDGE_LOOP ( 'NONE', ( #6557, #1390, #5045, #2701 ) ) ;
#11127 = EDGE_LOOP ( 'NONE', ( #6607, #10313, #10963, #2851 ) ) ;
#11128 = DIRECTION ( 'NONE',  ( 0.000000000000000000, 1.530455820933490821E-32, -1.000000000000000000 ) ) ;
#11129 = CARTESIAN_POINT ( 'NONE',  ( 0.000000000000000000, 0.000000000000000000, 3.469446951953614189E-15 ) ) ;
#11130 = ORIENTED_EDGE ( 'NONE', *, *, #6317, .T. ) ;
#11131 = CARTESIAN_POINT ( 'NONE',  ( 20.00000000000000000, 22.56100271565320625, -6.249672610153678143 ) ) ;
#11132 = VERTEX_POINT ( 'NONE', #9676 ) ;
#11133 = DIRECTION ( 'NONE',  ( -1.000000000000000000, -1.031065855027150586E-29, 2.218671295934095703E-30 ) ) ;
#11134 = DIRECTION ( 'NONE',  ( 1.000000000000000000, -1.010728034814421376E-30, -1.090846720500930387E-30 ) ) ;
#11135 = EDGE_CURVE ( 'NONE', #2451, #6872, #6568, .T. ) ;
#11136 = DIRECTION ( 'NONE',  ( 0.000000000000000000, -0.4338837391175658365, 0.9009688679024154823 ) ) ;
#11137 = ADVANCED_FACE ( 'NONE', ( #11694 ), #5829, .F. ) ;
#11138 = EDGE_CURVE ( 'NONE', #1463, #7479, #10240, .T. ) ;
#11139 = CARTESIAN_POINT ( 'NONE',  ( 3.054370817402604524E-30, 6.544726022087268724, 2.140719964816360399 ) ) ;
#11140 = ORIENTED_EDGE ( 'NONE', *, *, #3359, .F. ) ;
#11142 = DIRECTION ( 'NONE',  ( -1.000000000000000000, 6.162975822039154730E-33, 4.563833282352349791E-17 ) ) ;
#11141 = CIRCLE ( 'NONE', #6827, 6.499000000000006771 ) ;
#11143 = ORIENTED_EDGE ( 'NONE', *, *, #3531, .F. ) ;
#11144 = CYLINDRICAL_SURFACE ( 'NONE', #10106, 2.149999999999992362 ) ;
#11145 = ADVANCED_FACE ( 'NONE', ( #10845 ), #10973, .F. ) ;
#11146 = SURFACE_STYLE_FILL_AREA ( #11210 ) ;
#11147 = DIRECTION ( 'NONE',  ( 1.000000000000000000, 1.081682119347366321E-16, -5.551115123125780237E-17 ) ) ;
#11148 = VECTOR ( 'NONE', #7919, 999.9999999999998863 ) ;
#11149 = CARTESIAN_POINT ( 'NONE',  ( 15.00000000000003375, -12.49999999999999645, 3.994800001834461867E-31 ) ) ;
#11150 = AXIS2_PLACEMENT_3D ( 'NONE', #7673, #10684, #1746 ) ;
#11151 = CARTESIAN_POINT ( 'NONE',  ( 4.000000000000001776, -2.511475576507302687, -3.469253905236651558 ) ) ;
#11152 = CARTESIAN_POINT ( 'NONE',  ( 21.00000000000004974, -12.49999999999999289, 5.000000000000007994 ) ) ;
#11153 = CARTESIAN_POINT ( 'NONE',  ( 0.1999999999999987899, 0.000000000000000000, 3.499999999999982681 ) ) ;
#11154 = VERTEX_POINT ( 'NONE', #1121 ) ;
#11155 = DIRECTION ( 'NONE',  ( -1.000000000000000000, 1.010728034814421376E-30, 1.090846720500930387E-30 ) ) ;
#11156 = CARTESIAN_POINT ( 'NONE',  ( 32.99999999999999289, 39.49790820824818383, -24.06186359251417883 ) ) ;
#11157 = AXIS2_PLACEMENT_3D ( 'NONE', #8556, #3734, #5535 ) ;
#11158 = ADVANCED_FACE ( 'NONE', ( #4993 ), #9036, .T. ) ;
#11159 = ORIENTED_EDGE ( 'NONE', *, *, #5020, .T. ) ;
#11160 = DIRECTION ( 'NONE',  ( -1.000000000000000000, 0.000000000000000000, 0.000000000000000000 ) ) ;
#11161 = CARTESIAN_POINT ( 'NONE',  ( 20.00000000000000000, 16.67945018363952059, -6.690790236289298143 ) ) ;
#11162 = CYLINDRICAL_SURFACE ( 'NONE', #4262, 2.149999999999999023 ) ;
#11163 = DIRECTION ( 'NONE',  ( 1.000000000000000000, 0.000000000000000000, 0.000000000000000000 ) ) ;
#11164 = AXIS2_PLACEMENT_3D ( 'NONE', #8508, #6528, #3631 ) ;
#11165 = DIRECTION ( 'NONE',  ( -1.000000000000000000, 1.006188713385347367E-17, 3.844790828812615713E-17 ) ) ;
#11166 = AXIS2_PLACEMENT_3D ( 'NONE', #11653, #5475, #9379 ) ;
#11167 = ADVANCED_FACE ( 'NONE', ( #10059 ), #3017, .T. ) ;
#11168 = CARTESIAN_POINT ( 'NONE',  ( 0.000000000000000000, 2.918117354836734290, -5.807029542149833468 ) ) ;
#11169 = EDGE_CURVE ( 'NONE', #1828, #3396, #1208, .T. ) ;
#11170 = SURFACE_SIDE_STYLE ('',( #7371 ) ) ;
#11171 = ORIENTED_EDGE ( 'NONE', *, *, #9031, .T. ) ;
#11172 = PLANE ( 'NONE',  #845 ) ;
#11173 = EDGE_LOOP ( 'NONE', ( #10350, #8588, #8489, #7897 ) ) ;
#11174 = AXIS2_PLACEMENT_3D ( 'NONE', #3463, #9476, #547 ) ;
#11175 = VERTEX_POINT ( 'NONE', #95 ) ;
#11176 = ORIENTED_EDGE ( 'NONE', *, *, #7732, .F. ) ;
#11177 = DIRECTION ( 'NONE',  ( 0.000000000000000000, -0.3513748240813304724, -0.9362348706397417564 ) ) ;
#11178 = LINE ( 'NONE', #1382, #1711 ) ;
#11179 = CARTESIAN_POINT ( 'NONE',  ( 3.054370817402604524E-30, 6.557268578288196537, 3.319920822022213613 ) ) ;
#11180 = CYLINDRICAL_SURFACE ( 'NONE', #5109, 4.000000000000000000 ) ;
#11181 = DIRECTION ( 'NONE',  ( -1.000000000000000000, 0.000000000000000000, 0.000000000000000000 ) ) ;
#11182 = ORIENTED_EDGE ( 'NONE', *, *, #1282, .F. ) ;
#11183 = CARTESIAN_POINT ( 'NONE',  ( -0.6640947660594385127, 4.471078309994347855, -3.602146406945782253 ) ) ;
#11184 = EDGE_CURVE ( 'NONE', #5073, #9626, #3343, .T. ) ;
#11185 = CIRCLE ( 'NONE', #4394, 3.299999999999999822 ) ;
#11186 = CARTESIAN_POINT ( 'NONE',  ( 32.99999999999999289, 39.34792583643766051, -17.06347054209567915 ) ) ;
#11187 = EDGE_LOOP ( 'NONE', ( #8408, #565, #2912, #10517 ) ) ;
#11188 = ORIENTED_EDGE ( 'NONE', *, *, #2925, .T. ) ;
#11189 = EDGE_CURVE ( 'NONE', #4626, #5504, #443, .T. ) ;
#11190 = VERTEX_POINT ( 'NONE', #5118 ) ;
#11191 = ORIENTED_EDGE ( 'NONE', *, *, #6846, .F. ) ;
#11192 = DIRECTION ( 'NONE',  ( 0.000000000000000000, -1.000000000000000000, 0.000000000000000000 ) ) ;
#11193 = EDGE_CURVE ( 'NONE', #10862, #8204, #5991, .T. ) ;
#11194 = AXIS2_PLACEMENT_3D ( 'NONE', #3385, #6261, #10304 ) ;
#11195 =( LENGTH_UNIT ( ) NAMED_UNIT ( * ) SI_UNIT ( .MILLI., .METRE. ) );
#11196 = ORIENTED_EDGE ( 'NONE', *, *, #6225, .F. ) ;
#11197 = CARTESIAN_POINT ( 'NONE',  ( 19.99999999999999645, -5.148708580507647348, -3.965829163366334953 ) ) ;
#11198 = EDGE_LOOP ( 'NONE', ( #9506, #3458, #8016, #3295 ) ) ;
#11199 = CARTESIAN_POINT ( 'NONE',  ( -3.510273485745275313, -2.827716139362673964, -3.610536846335894889 ) ) ;
#11200 = DIRECTION ( 'NONE',  ( 1.000000000000000000, 0.000000000000000000, 0.000000000000000000 ) ) ;
#11201 = AXIS2_PLACEMENT_3D ( 'NONE', #1957, #7051, #2089 ) ;
#11202 = DIRECTION ( 'NONE',  ( -1.000000000000000000, 1.010728034814421376E-30, 1.090846720500930387E-30 ) ) ;
#11203 = PRODUCT_DEFINITION_CONTEXT ( 'detailed design', #9204, 'design' ) ;
#11204 = EDGE_CURVE ( 'NONE', #9165, #8354, #9069, .T. ) ;
#11205 = DIRECTION ( 'NONE',  ( 1.238279320584846685E-16, -0.9554649393887558739, 0.2951046417778634412 ) ) ;
#11206 = VERTEX_POINT ( 'NONE', #3962 ) ;
#11207 = ORIENTED_EDGE ( 'NONE', *, *, #3878, .F. ) ;
#11208 = DIRECTION ( 'NONE',  ( -1.000000000000000000, 1.010728034814421376E-30, 1.090846720500930387E-30 ) ) ;
#11209 = VECTOR ( 'NONE', #6315, 1000.000000000000000 ) ;
#11210 = FILL_AREA_STYLE ('',( #7285 ) ) ;
#11211 = ADVANCED_FACE ( 'NONE', ( #12017 ), #7884, .T. ) ;
#11212 = DIRECTION ( 'NONE',  ( 1.000000000000000000, 0.000000000000000000, 0.000000000000000000 ) ) ;
#11213 = EDGE_CURVE ( 'NONE', #35, #6322, #11347, .T. ) ;
#11214 = DIRECTION ( 'NONE',  ( -1.000000000000000000, 1.010728034814421376E-30, 1.090846720500930387E-30 ) ) ;
#11215 = EDGE_CURVE ( 'NONE', #9645, #4775, #5780, .T. ) ;
#11216 = PRODUCT ( 'fixed position lower roller', 'fixed position lower roller', '', ( #8072 ) ) ;
#11217 = CARTESIAN_POINT ( 'NONE',  ( 9.999999999999998224, 5.914787828628609745, -4.446941076999683773 ) ) ;
#11218 = DIRECTION ( 'NONE',  ( 0.000000000000000000, 0.000000000000000000, -1.000000000000000000 ) ) ;
#11219 = AXIS2_PLACEMENT_3D ( 'NONE', #4115, #8238, #1210 ) ;
#11220 = AXIS2_PLACEMENT_3D ( 'NONE', #5513, #8404, #2698 ) ;
#11221 = CARTESIAN_POINT ( 'NONE',  ( 19.99999999999999645, 5.280167904461726458, 3.922743398397384063 ) ) ;
#11222 = ORIENTED_EDGE ( 'NONE', *, *, #978, .T. ) ;
#11223 = CARTESIAN_POINT ( 'NONE',  ( 0.000000000000000000, 4.494880553659021061, 4.802513683199234329 ) ) ;
#11224 = DIRECTION ( 'NONE',  ( -1.000000000000000000, 1.010728034814421376E-30, 1.090846720500930387E-30 ) ) ;
#11225 = EDGE_CURVE ( 'NONE', #6170, #9393, #4931, .T. ) ;
#11226 = ORIENTED_EDGE ( 'NONE', *, *, #6814, .T. ) ;
#11227 = VECTOR ( 'NONE', #11165, 1000.000000000000000 ) ;
#11228 = LINE ( 'NONE', #4265, #11588 ) ;
#11229 = LINE ( 'NONE', #4331, #12225 ) ;
#11230 = CARTESIAN_POINT ( 'NONE',  ( 33.00000000000001421, 81.84122341717352356, -27.68198508464163510 ) ) ;
#11231 = CARTESIAN_POINT ( 'NONE',  ( 19.99999999999997868, -2.720702104306968572, -5.902099716170495114 ) ) ;
#11232 = DIRECTION ( 'NONE',  ( 1.000000000000000000, 1.081682119347366197E-16, -6.938893903907228378E-17 ) ) ;
#11233 = DIRECTION ( 'NONE',  ( -1.392832535780847042E-30, 0.8345732537212999791, 0.5508969814521064157 ) ) ;
#11234 = EDGE_CURVE ( 'NONE', #4694, #1828, #8988, .T. ) ;
#11235 = FILL_AREA_STYLE_COLOUR ( '', #12133 ) ;
#11236 = ORIENTED_EDGE ( 'NONE', *, *, #3565, .F. ) ;
#11237 = CARTESIAN_POINT ( 'NONE',  ( -4.101948962586056346, 2.368261337751164763, -3.681124513963754730 ) ) ;
#11238 = ORIENTED_EDGE ( 'NONE', *, *, #8206, .F. ) ;
#11239 = ORIENTED_EDGE ( 'NONE', *, *, #11924, .F. ) ;
#11240 = ORIENTED_EDGE ( 'NONE', *, *, #3183, .T. ) ;
#11241 = EDGE_CURVE ( 'NONE', #4279, #7331, #1051, .T. ) ;
#11242 = CARTESIAN_POINT ( 'NONE',  ( 34.00000000000000000, 0.000000000000000000, 1.609999999999982778 ) ) ;
#11243 = EDGE_CURVE ( 'NONE', #10795, #7388, #3541, .T. ) ;
#11244 = SURFACE_STYLE_FILL_AREA ( #8147 ) ;
#11245 = FACE_OUTER_BOUND ( 'NONE', #2876, .T. ) ;
#11246 = VECTOR ( 'NONE', #6094, 1000.000000000000000 ) ;
#11247 = DIRECTION ( 'NONE',  ( -7.062770292056861511E-30, -0.4999999999999991673, 0.8660254037844392627 ) ) ;
#11248 = VERTEX_POINT ( 'NONE', #7251 ) ;
#11249 = AXIS2_PLACEMENT_3D ( 'NONE', #548, #734, #2494 ) ;
#11250 = LINE ( 'NONE', #7384, #5046 ) ;
#11251 = EDGE_CURVE ( 'NONE', #1961, #4493, #4275, .T. ) ;
#11252 = CARTESIAN_POINT ( 'NONE',  ( 33.00000000000000711, 39.92642927056392210, -44.05727230799563898 ) ) ;
#11253 = ORIENTED_EDGE ( 'NONE', *, *, #12415, .T. ) ;
#11254 = ORIENTED_EDGE ( 'NONE', *, *, #2247, .T. ) ;
#11255 = ORIENTED_EDGE ( 'NONE', *, *, #6317, .F. ) ;
#11256 = AXIS2_PLACEMENT_3D ( 'NONE', #2787, #6702, #10612 ) ;
#11257 = ORIENTED_EDGE ( 'NONE', *, *, #3563, .T. ) ;
#11258 = AXIS2_PLACEMENT_3D ( 'NONE', #7745, #1690, #2869 ) ;
#11259 = CARTESIAN_POINT ( 'NONE',  ( 14.00000000000000000, -12.99999999999999822, 4.000000000000000000 ) ) ;
#11260 = AXIS2_PLACEMENT_3D ( 'NONE', #11674, #11805, #8825 ) ;
#11261 = ADVANCED_BREP_SHAPE_REPRESENTATION ( '', ( #9919, #12422 ), #3113 ) ;
#11262 = CARTESIAN_POINT ( 'NONE',  ( 40.00000000000000711, 18.52447679111068268, -16.77732469694377926 ) ) ;
#11263 = ORIENTED_EDGE ( 'NONE', *, *, #11204, .F. ) ;
#11264 = DIRECTION ( 'NONE',  ( -1.000000000000000000, -1.031065855027150586E-29, 2.218671295934095703E-30 ) ) ;
#11265 = ORIENTED_EDGE ( 'NONE', *, *, #6371, .F. ) ;
#11266 = DIRECTION ( 'NONE',  ( 1.140150527077241873E-30, 0.000000000000000000, -1.000000000000000000 ) ) ;
#11267 = LINE ( 'NONE', #10278, #11418 ) ;
#11268 = AXIS2_PLACEMENT_3D ( 'NONE', #4287, #1135, #10071 ) ;
#11269 = DIRECTION ( 'NONE',  ( -1.000000000000000000, 1.010728034814421376E-30, 1.090846720500930387E-30 ) ) ;
#11270 = CARTESIAN_POINT ( 'NONE',  ( 32.99999999999999289, 39.34792583643765340, -17.06347054209567560 ) ) ;
#11271 = ORIENTED_EDGE ( 'NONE', *, *, #7433, .F. ) ;
#11272 = EDGE_LOOP ( 'NONE', ( #8746, #6560, #12545, #11696, #10126, #1071, #5061, #5713 ) ) ;
#11273 = DIRECTION ( 'NONE',  ( 1.000000000000000000, 1.081682119347366197E-16, -6.938893903907228378E-17 ) ) ;
#11274 =( NAMED_UNIT ( * ) SI_UNIT ( $, .STERADIAN. ) SOLID_ANGLE_UNIT ( ) );
#11275 = DIRECTION ( 'NONE',  ( 0.000000000000000000, 0.000000000000000000, 1.000000000000000000 ) ) ;
#11276 = CYLINDRICAL_SURFACE ( 'NONE', #2801, 6.000000000000000000 ) ;
#11277 = DIRECTION ( 'NONE',  ( 1.000000000000000000, 1.849040895279789448E-31, -6.938893903907224680E-17 ) ) ;
#11278 = DIRECTION ( 'NONE',  ( 0.000000000000000000, 0.000000000000000000, -1.000000000000000000 ) ) ;
#11279 = CARTESIAN_POINT ( 'NONE',  ( -18.00000000000002842, 30.00000000000000000, 1.369224906555730040E-16 ) ) ;
#11280 = ADVANCED_FACE ( 'NONE', ( #3578, #12404 ), #1373, .T. ) ;
#11281 = VERTEX_POINT ( 'NONE', #5368 ) ;
#11282 = DIRECTION ( 'NONE',  ( 4.606824426974262030E-31, 0.5128992774059070170, -0.8584487936018656562 ) ) ;
#11283 = LINE ( 'NONE', #2468, #7656 ) ;
#11284 =( LENGTH_UNIT ( ) NAMED_UNIT ( * ) SI_UNIT ( .MILLI., .METRE. ) );
#11285 = ORIENTED_EDGE ( 'NONE', *, *, #7036, .T. ) ;
#11286 = CARTESIAN_POINT ( 'NONE',  ( 40.00000000000000711, 18.52447679111068268, -16.77732469694377926 ) ) ;
#11287 = CARTESIAN_POINT ( 'NONE',  ( 15.00000000000003375, -12.49999999999999645, -4.000000000000000000 ) ) ;
#11288 = AXIS2_PLACEMENT_3D ( 'NONE', #6981, #6798, #5883 ) ;
#11289 = CYLINDRICAL_SURFACE ( 'NONE', #11670, 2.800000000000003819 ) ;
#11290 = CARTESIAN_POINT ( 'NONE',  ( 2.000000000000001776, 1.773042676681338303, 0.000000000000000000 ) ) ;
#11291 = LINE ( 'NONE', #3573, #1547 ) ;
#11292 = DIRECTION ( 'NONE',  ( -1.000000000000000000, 1.010728034814421376E-30, 1.090846720500930387E-30 ) ) ;
#11293 = EDGE_CURVE ( 'NONE', #3082, #4276, #4765, .T. ) ;
#11294 = DIRECTION ( 'NONE',  ( 0.000000000000000000, -0.2951046417778627751, -0.9554649393887560960 ) ) ;
#11295 = AXIS2_PLACEMENT_3D ( 'NONE', #263, #6062, #1166 ) ;
#11296 = CIRCLE ( 'NONE', #11507, 0.5155456020628804703 ) ;
#11297 = VERTEX_POINT ( 'NONE', #4406 ) ;
#11298 = DIRECTION ( 'NONE',  ( -1.000000000000000000, 0.000000000000000000, 0.000000000000000000 ) ) ;
#11299 = ORIENTED_EDGE ( 'NONE', *, *, #10226, .F. ) ;
#11300 = AXIS2_PLACEMENT_3D ( 'NONE', #9045, #7125, #289 ) ;
#11301 = EDGE_LOOP ( 'NONE', ( #6953, #9820, #10556, #7522 ) ) ;
#11302 = ADVANCED_FACE ( 'NONE', ( #5305 ), #12275, .T. ) ;
#11303 = ORIENTED_EDGE ( 'NONE', *, *, #7003, .F. ) ;
#11304 = ORIENTED_EDGE ( 'NONE', *, *, #2979, .T. ) ;
#11305 = CARTESIAN_POINT ( 'NONE',  ( 0.000000000000000000, 0.000000000000000000, -0.2800830152838839626 ) ) ;
#11306 = VECTOR ( 'NONE', #1214, 1000.000000000000000 ) ;
#11307 = CARTESIAN_POINT ( 'NONE',  ( 11.00000000000001599, 19.99999999999999645, 9.850000000000035172 ) ) ;
#11308 = FACE_OUTER_BOUND ( 'NONE', #1054, .T. ) ;
#11309 = AXIS2_PLACEMENT_3D ( 'NONE', #6602, #11493, #1817 ) ;
#11310 = CIRCLE ( 'NONE', #12551, 2.800000000000002931 ) ;
#11311 = CARTESIAN_POINT ( 'NONE',  ( 19.99999999999997868, 6.057062246029579100, -4.251117141143414990 ) ) ;
#11312 = ORIENTED_EDGE ( 'NONE', *, *, #1676, .T. ) ;
#11313 = CARTESIAN_POINT ( 'NONE',  ( 0.000000000000000000, 5.012092988313943565, 4.137139697483554812 ) ) ;
#11314 = AXIS2_PLACEMENT_3D ( 'NONE', #6153, #12094, #10130 ) ;
#11315 = EDGE_CURVE ( 'NONE', #11905, #9583, #11141, .T. ) ;
#11316 = CARTESIAN_POINT ( 'NONE',  ( 19.99999999999999645, 0.000000000000000000, 0.000000000000000000 ) ) ;
#11317 = ORIENTED_EDGE ( 'NONE', *, *, #9642, .T. ) ;
#11318 = ADVANCED_FACE ( 'NONE', ( #5503 ), #9268, .T. ) ;
#11319 = ORIENTED_EDGE ( 'NONE', *, *, #7277, .F. ) ;
#11320 = VERTEX_POINT ( 'NONE', #2487 ) ;
#11321 = EDGE_CURVE ( 'NONE', #38, #3396, #5007, .T. ) ;
#11322 = AXIS2_PLACEMENT_3D ( 'NONE', #12416, #4290, #8219 ) ;
#11323 = EDGE_LOOP ( 'NONE', ( #2768, #3772, #427, #4640 ) ) ;
#11324 = VECTOR ( 'NONE', #4260, 1000.000000000000000 ) ;
#11325 = VECTOR ( 'NONE', #1809, 1000.000000000000000 ) ;
#11326 = CARTESIAN_POINT ( 'NONE',  ( 2.000000000000001776, 3.469446951953614189E-15, 1.535499999999998755 ) ) ;
#11327 = ORIENTED_EDGE ( 'NONE', *, *, #8531, .T. ) ;
#11328 = ADVANCED_FACE ( 'NONE', ( #11432 ), #2510, .F. ) ;
#11329 = DIRECTION ( 'NONE',  ( 1.000000000000000000, -1.010728034814421376E-30, -1.090846720500930387E-30 ) ) ;
#11330 = EDGE_LOOP ( 'NONE', ( #10197, #9993, #8364, #9054 ) ) ;
#11331 = CARTESIAN_POINT ( 'NONE',  ( 33.00000000000001421, 39.34792583643766761, -24.06347054209567915 ) ) ;
#11332 = CARTESIAN_POINT ( 'NONE',  ( 11.00000000000003375, -19.99999999999999645, 9.850000000000035172 ) ) ;
#11333 = MECHANICAL_DESIGN_GEOMETRIC_PRESENTATION_REPRESENTATION (  '', ( #4332 ), #8853 ) ;
#11334 = VECTOR ( 'NONE', #11953, 1000.000000000000000 ) ;
#11335 = DIRECTION ( 'NONE',  ( -1.000000000000000000, 1.010728034814421376E-30, 1.090846720500930387E-30 ) ) ;
#11336 = ADVANCED_FACE ( 'NONE', ( #543 ), #4342, .T. ) ;
#11337 = DIRECTION ( 'NONE',  ( -0.000000000000000000, -0.000000000000000000, -1.000000000000000000 ) ) ;
#11338 = EDGE_CURVE ( 'NONE', #5523, #7377, #1568, .T. ) ;
#11339 = EDGE_LOOP ( 'NONE', ( #1056, #6418, #5704, #885 ) ) ;
#11340 = VERTEX_POINT ( 'NONE', #7313 ) ;
#11341 = LINE ( 'NONE', #511, #460 ) ;
#11342 =( GEOMETRIC_REPRESENTATION_CONTEXT ( 3 ) GLOBAL_UNCERTAINTY_ASSIGNED_CONTEXT ( ( #12560 ) ) GLOBAL_UNIT_ASSIGNED_CONTEXT ( ( #7410, #2526, #1540 ) ) REPRESENTATION_CONTEXT ( 'NONE', 'WORKASPACE' ) );
#11343 = CARTESIAN_POINT ( 'NONE',  ( 20.00000000000000355, 18.52447679111067913, -16.77732469694377926 ) ) ;
#11344 = DIRECTION ( 'NONE',  ( 1.084202172485504434E-16, 0.000000000000000000, 1.000000000000000000 ) ) ;
#11345 = CARTESIAN_POINT ( 'NONE',  ( 0.000000000000000000, -6.577476285968332448, 0.06996125000490599488 ) ) ;
#11346 = DIRECTION ( 'NONE',  ( -1.000000000000000000, 1.010728034814421376E-30, 1.090846720500930387E-30 ) ) ;
#11347 = CIRCLE ( 'NONE', #2730, 7.400000000000011902 ) ;
#11348 = DIRECTION ( 'NONE',  ( 0.000000000000000000, 0.000000000000000000, -1.000000000000000000 ) ) ;
#11349 = EDGE_LOOP ( 'NONE', ( #12576, #7311, #1375, #5813 ) ) ;
#11350 = CARTESIAN_POINT ( 'NONE',  ( 1.390230914382213800, 4.043987460488878583, -3.502507215260568962 ) ) ;
#11351 = DIRECTION ( 'NONE',  ( -1.000000000000000000, 1.010728034814421376E-30, 1.090846720500930387E-30 ) ) ;
#11352 = ADVANCED_FACE ( 'NONE', ( #347 ), #11172, .F. ) ;
#11353 = SURFACE_STYLE_FILL_AREA ( #526 ) ;
#11354 = ADVANCED_FACE ( 'NONE', ( #12213 ), #3517, .T. ) ;
#11355 = DIRECTION ( 'NONE',  ( 1.000000000000000000, -1.010728034814421376E-30, -1.090846720500930387E-30 ) ) ;
#11356 = CIRCLE ( 'NONE', #2738, 6.999999999999999112 ) ;
#11357 = ORIENTED_EDGE ( 'NONE', *, *, #10281, .T. ) ;
#11358 = CARTESIAN_POINT ( 'NONE',  ( 0.000000000000000000, 0.000000000000000000, 0.000000000000000000 ) ) ;
#11359 = CARTESIAN_POINT ( 'NONE',  ( 0.000000000000000000, 0.000000000000000000, 0.000000000000000000 ) ) ;
#11360 = CARTESIAN_POINT ( 'NONE',  ( 1.312671235360366895, 3.860931062424212801, -0.05923475698269817236 ) ) ;
#11361 = CARTESIAN_POINT ( 'NONE',  ( 0.000000000000000000, -3.055252325922142020, -5.825248672282193674 ) ) ;
#11362 = CARTESIAN_POINT ( 'NONE',  ( 0.000000000000000000, -4.155687294075552707, -5.098857909653597531 ) ) ;
#11363 = DIRECTION ( 'NONE',  ( 1.140150527077241873E-30, 0.000000000000000000, -1.000000000000000000 ) ) ;
#11364 = VECTOR ( 'NONE', #2131, 1000.000000000000000 ) ;
#11365 = PRESENTATION_STYLE_ASSIGNMENT (( #2355 ) ) ;
#11366 = CARTESIAN_POINT ( 'NONE',  ( 33.00000000000001421, 81.84122341717352356, -27.68198508464163510 ) ) ;
#11367 = ORIENTED_EDGE ( 'NONE', *, *, #6655, .F. ) ;
#11368 = CONTEXT_DEPENDENT_SHAPE_REPRESENTATION ( #169, #6989 ) ;
#11369 = ORIENTED_EDGE ( 'NONE', *, *, #9913, .F. ) ;
#11370 = ORIENTED_EDGE ( 'NONE', *, *, #10009, .T. ) ;
#11371 = AXIS2_PLACEMENT_3D ( 'NONE', #6461, #9337, #8385 ) ;
#11372 = EDGE_CURVE ( 'NONE', #11435, #93, #2932, .T. ) ;
#11373 = DIRECTION ( 'NONE',  ( -1.000000000000000000, 1.010728034814421376E-30, 1.090846720500930387E-30 ) ) ;
#11374 = EDGE_CURVE ( 'NONE', #7142, #2431, #11618, .T. ) ;
#11375 = DIRECTION ( 'NONE',  ( 0.000000000000000000, 0.000000000000000000, 1.000000000000000000 ) ) ;
#11377 = EDGE_CURVE ( 'NONE', #11114, #8922, #234, .T. ) ;
#11376 = CARTESIAN_POINT ( 'NONE',  ( 33.00000000000000711, 39.92642927056392210, -44.05727230799563898 ) ) ;
#11378 = LINE ( 'NONE', #1642, #2191 ) ;
#11379 = EDGE_LOOP ( 'NONE', ( #2557, #4744, #9196, #10023 ) ) ;
#11380 = CARTESIAN_POINT ( 'NONE',  ( 19.99999999999997868, 6.146182963951697609, -2.112211157443803611 ) ) ;
#11381 = DIRECTION ( 'NONE',  ( 2.206481006425900381E-16, -1.000000000000000000, 0.000000000000000000 ) ) ;
#11382 = ORIENTED_EDGE ( 'NONE', *, *, #6239, .F. ) ;
#11383 = AXIS2_PLACEMENT_3D ( 'NONE', #12090, #2031, #4089 ) ;
#11384 = ORIENTED_EDGE ( 'NONE', *, *, #9033, .F. ) ;
#11385 = LINE ( 'NONE', #3533, #3884 ) ;
#11386 = ORIENTED_EDGE ( 'NONE', *, *, #12590, .F. ) ;
#11387 = VECTOR ( 'NONE', #5323, 1000.000000000000227 ) ;
#11388 = VERTEX_POINT ( 'NONE', #7625 ) ;
#11389 = SURFACE_STYLE_FILL_AREA ( #5585 ) ;
#11390 = ORIENTED_EDGE ( 'NONE', *, *, #10167, .T. ) ;
#11391 = CARTESIAN_POINT ( 'NONE',  ( 19.99999999999999645, -6.459281472512932609, -1.243290685169442966 ) ) ;
#11392 = CARTESIAN_POINT ( 'NONE',  ( 27.00000000000001421, 81.84122341717352356, -12.68198508464164931 ) ) ;
#11393 = VERTEX_POINT ( 'NONE', #11495 ) ;
#11394 = AXIS2_PLACEMENT_3D ( 'NONE', #1429, #10229, #7428 ) ;
#11395 = EDGE_CURVE ( 'NONE', #12687, #2961, #11561, .T. ) ;
#11396 = DIRECTION ( 'NONE',  ( -1.000000000000000000, 0.000000000000000000, 0.000000000000000000 ) ) ;
#11397 = DIRECTION ( 'NONE',  ( -4.930380657631325535E-31, -1.000000000000000000, -1.177425296209239362E-30 ) ) ;
#11398 = DIRECTION ( 'NONE',  ( 0.000000000000000000, -1.530455820933490821E-32, 1.000000000000000000 ) ) ;
#11399 = UNCERTAINTY_MEASURE_WITH_UNIT (LENGTH_MEASURE( 1.000000000000000082E-05 ), #255, 'distance_accuracy_value', 'NONE');
#11400 = DIRECTION ( 'NONE',  ( -1.000000000000000000, 1.010728034814421376E-30, 1.090846720500930387E-30 ) ) ;
#11401 = EDGE_CURVE ( 'NONE', #7234, #2472, #2090, .T. ) ;
#11402 = ORIENTED_EDGE ( 'NONE', *, *, #10219, .T. ) ;
#11403 = AXIS2_PLACEMENT_3D ( 'NONE', #2673, #4594, #5801 ) ;
#11404 = ORIENTED_EDGE ( 'NONE', *, *, #11963, .F. ) ;
#11405 = CARTESIAN_POINT ( 'NONE',  ( -18.00000000000002842, 30.00000000000000000, 1.369224906555730040E-16 ) ) ;
#11406 = DIRECTION ( 'NONE',  ( 0.000000000000000000, 0.000000000000000000, 1.000000000000000000 ) ) ;
#11407 = CARTESIAN_POINT ( 'NONE',  ( 0.1999999999999987899, 0.000000000000000000, -1.734723475976807094E-14 ) ) ;
#11408 = EDGE_CURVE ( 'NONE', #4169, #87, #1884, .T. ) ;
#11409 = VECTOR ( 'NONE', #10119, 1000.000000000000000 ) ;
#11410 = CYLINDRICAL_SURFACE ( 'NONE', #7309, 2.800000000000003819 ) ;
#11411 = EDGE_CURVE ( 'NONE', #6027, #4169, #10090, .T. ) ;
#11412 = VECTOR ( 'NONE', #7836, 1000.000000000000000 ) ;
#11413 = DIRECTION ( 'NONE',  ( 1.000000000000000000, -1.010728034814421376E-30, -1.090846720500930387E-30 ) ) ;
#11414 = DIRECTION ( 'NONE',  ( 0.000000000000000000, 1.530455820933490821E-32, -1.000000000000000000 ) ) ;
#11415 = ORIENTED_EDGE ( 'NONE', *, *, #10429, .F. ) ;
#11416 = DIRECTION ( 'NONE',  ( -1.000000000000000000, 1.010728034814421376E-30, 1.090846720500930387E-30 ) ) ;
#11417 = CIRCLE ( 'NONE', #8135, 2.800000000000003819 ) ;
#11418 = VECTOR ( 'NONE', #5397, 1000.000000000000000 ) ;
#11419 = CARTESIAN_POINT ( 'NONE',  ( 0.000000000000000000, -3.469446951953614189E-14, -25.03750572909320837 ) ) ;
#11420 = DIRECTION ( 'NONE',  ( -1.000000000000000000, 1.010728034814421376E-30, 1.090846720500930387E-30 ) ) ;
#11421 = ORIENTED_EDGE ( 'NONE', *, *, #9689, .F. ) ;
#11422 = DIRECTION ( 'NONE',  ( 1.000000000000000000, 1.081682119347366321E-16, -5.551115123125780237E-17 ) ) ;
#11423 = DIRECTION ( 'NONE',  ( -3.437775699846489820E-17, -0.2951046417778627751, -0.9554649393887560960 ) ) ;
#11425 = CARTESIAN_POINT ( 'NONE',  ( 0.000000000000000000, 2.649444137877682515, -6.020675595748679498 ) ) ;
#11424 = VECTOR ( 'NONE', #9766, 1000.000000000000000 ) ;
#11426 = FACE_OUTER_BOUND ( 'NONE', #3211, .T. ) ;
#11427 = CIRCLE ( 'NONE', #4641, 4.000000000000000000 ) ;
#11428 = PLANE ( 'NONE',  #11019 ) ;
#11429 = DIRECTION ( 'NONE',  ( 1.503766100577550951E-30, -0.7818314824680222541, -0.6234898018587429203 ) ) ;
#11430 = EDGE_CURVE ( 'NONE', #2832, #9185, #6195, .T. ) ;
#11431 = DIRECTION ( 'NONE',  ( 0.000000000000000000, 0.000000000000000000, 1.000000000000000000 ) ) ;
#11432 = FACE_OUTER_BOUND ( 'NONE', #8233, .T. ) ;
#11433 = VERTEX_POINT ( 'NONE', #917 ) ;
#11434 = CIRCLE ( 'NONE', #8345, 4.000000000000000000 ) ;
#11435 = VERTEX_POINT ( 'NONE', #12526 ) ;
#11436 = ORIENTED_EDGE ( 'NONE', *, *, #5020, .F. ) ;
#11437 = DIRECTION ( 'NONE',  ( 1.000000000000000000, 1.081682119347366197E-16, -6.938893903907228378E-17 ) ) ;
#11438 = DIRECTION ( 'NONE',  ( -2.465190328815656418E-32, 1.177425296209236734E-30, 1.000000000000000000 ) ) ;
#11439 = DIRECTION ( 'NONE',  ( 0.7071067811865504593, 0.000000000000000000, 0.7071067811865445751 ) ) ;
#11440 = DIRECTION ( 'NONE',  ( -1.000000000000000000, 1.010728034814421376E-30, 1.090846720500930387E-30 ) ) ;
#11441 = ORIENTED_EDGE ( 'NONE', *, *, #1075, .T. ) ;
#11442 = CARTESIAN_POINT ( 'NONE',  ( 14.00000000000000000, -30.00000000000000000, 0.000000000000000000 ) ) ;
#11443 = CIRCLE ( 'NONE', #7905, 2.149999999999999023 ) ;
#11444 = DIRECTION ( 'NONE',  ( 1.000000000000000000, 1.081682119347366197E-16, -6.938893903907228378E-17 ) ) ;
#11445 = ORIENTED_EDGE ( 'NONE', *, *, #8987, .T. ) ;
#11446 = EDGE_LOOP ( 'NONE', ( #4819, #11041, #637, #7787 ) ) ;
#11447 = EDGE_CURVE ( 'NONE', #8175, #9943, #7846, .T. ) ;
#11448 = DIRECTION ( 'NONE',  ( 1.000000000000000000, 1.848892746611742259E-31, -1.154721252774410375E-34 ) ) ;
#11449 = ORIENTED_EDGE ( 'NONE', *, *, #3742, .T. ) ;
#11450 = EDGE_CURVE ( 'NONE', #1090, #7720, #1760, .T. ) ;
#11451 = ORIENTED_EDGE ( 'NONE', *, *, #3043, .F. ) ;
#11452 =( NAMED_UNIT ( * ) PLANE_ANGLE_UNIT ( ) SI_UNIT ( $, .RADIAN. ) );
#11453 = LINE ( 'NONE', #6556, #124 ) ;
#11454 = VERTEX_POINT ( 'NONE', #5686 ) ;
#11455 = CIRCLE ( 'NONE', #6725, 7.400000000000011902 ) ;
#11456 = CARTESIAN_POINT ( 'NONE',  ( 40.00000000000006395, 1.290960574571364216E-15, -20.00000000000000000 ) ) ;
#11457 = CIRCLE ( 'NONE', #5685, 2.149999999999992362 ) ;
#11458 = FACE_OUTER_BOUND ( 'NONE', #2364, .T. ) ;
#11459 = ORIENTED_EDGE ( 'NONE', *, *, #4328, .T. ) ;
#11460 = CARTESIAN_POINT ( 'NONE',  ( 1.655952806101427699, -3.662737355149048746, -1.169794851805551168E-14 ) ) ;
#11461 = DIRECTION ( 'NONE',  ( -1.000000000000000000, 1.010728034814421376E-30, 1.090846720500930387E-30 ) ) ;
#11462 = LINE ( 'NONE', #505, #2804 ) ;
#11463 = CIRCLE ( 'NONE', #1790, 7.999999999999998224 ) ;
#11464 = FACE_BOUND ( 'NONE', #10026, .T. ) ;
#11465 = VECTOR ( 'NONE', #7488, 1000.000000000000000 ) ;
#11466 = ORIENTED_EDGE ( 'NONE', *, *, #4483, .F. ) ;
#11467 = EDGE_CURVE ( 'NONE', #4885, #156, #664, .T. ) ;
#11468 = PRODUCT_RELATED_PRODUCT_CATEGORY ( 'part', '', ( #7209 ) ) ;
#11469 = ORIENTED_EDGE ( 'NONE', *, *, #4914, .F. ) ;
#11470 = LINE ( 'NONE', #9444, #12614 ) ;
#11471 = DIRECTION ( 'NONE',  ( -1.000000000000000000, 0.000000000000000000, -6.982962677686266711E-15 ) ) ;
#11472 = ORIENTED_EDGE ( 'NONE', *, *, #2076, .F. ) ;
#11473 = CARTESIAN_POINT ( 'NONE',  ( 19.99999999999997868, 6.544726022087268724, 2.140719964816360399 ) ) ;
#11474 = AXIS2_PLACEMENT_3D ( 'NONE', #12252, #11277, #12313 ) ;
#11475 = CARTESIAN_POINT ( 'NONE',  ( 19.99999999999999645, 0.000000000000000000, 0.000000000000000000 ) ) ;
#11476 = FACE_OUTER_BOUND ( 'NONE', #1324, .T. ) ;
#11477 = DIRECTION ( 'NONE',  ( -1.140150527077241873E-30, 0.000000000000000000, 1.000000000000000000 ) ) ;
#11478 = VERTEX_POINT ( 'NONE', #8654 ) ;
#11479 = CARTESIAN_POINT ( 'NONE',  ( 14.00000000000000000, 30.00000000000000000, 0.000000000000000000 ) ) ;
#11480 = EDGE_CURVE ( 'NONE', #1822, #8348, #12595, .T. ) ;
#11481 = DIRECTION ( 'NONE',  ( 0.000000000000000000, 0.000000000000000000, -1.000000000000000000 ) ) ;
#11482 = EDGE_CURVE ( 'NONE', #6132, #12737, #12654, .T. ) ;
#11483 =( NAMED_UNIT ( * ) SI_UNIT ( $, .STERADIAN. ) SOLID_ANGLE_UNIT ( ) );
#11484 = ADVANCED_FACE ( 'NONE', ( #1819 ), #7753, .F. ) ;
#11485 = CARTESIAN_POINT ( 'NONE',  ( 4.000000000000001776, -1.539567084929416296E-14, -3.142992957459251890 ) ) ;
#11486 = DIRECTION ( 'NONE',  ( 0.000000000000000000, 0.000000000000000000, 1.000000000000000000 ) ) ;
#11487 = EDGE_CURVE ( 'NONE', #8864, #499, #7239, .T. ) ;
#11488 = CARTESIAN_POINT ( 'NONE',  ( 19.99999999999999645, 4.596015818000074304, 4.705818469689523553 ) ) ;
#11489 = DIRECTION ( 'NONE',  ( -1.000000000000000000, 1.010728034814421376E-30, 1.090846720500930387E-30 ) ) ;
#11490 = CARTESIAN_POINT ( 'NONE',  ( 40.00000000000000711, 18.52447679111068268, -16.77732469694377926 ) ) ;
#11491 = CARTESIAN_POINT ( 'NONE',  ( 0.000000000000000000, -5.148708580507658006, -3.965829163366345167 ) ) ;
#11492 = CARTESIAN_POINT ( 'NONE',  ( 14.00000000000000000, -12.99999999999999822, 0.000000000000000000 ) ) ;
#11493 = DIRECTION ( 'NONE',  ( -0.000000000000000000, -1.000000000000000000, -0.000000000000000000 ) ) ;
#11494 = UNCERTAINTY_MEASURE_WITH_UNIT (LENGTH_MEASURE( 1.000000000000000082E-05 ), #1779, 'distance_accuracy_value', 'NONE');
#11495 = CARTESIAN_POINT ( 'NONE',  ( -2.499999999999966249, -3.469446951953614189E-15, -4.974600000000009459 ) ) ;
#11496 = ORIENTED_EDGE ( 'NONE', *, *, #10989, .T. ) ;
#11497 = AXIS2_PLACEMENT_3D ( 'NONE', #7443, #4549, #12535 ) ;
#11498 = VERTEX_POINT ( 'NONE', #1693 ) ;
#11499 = ORIENTED_EDGE ( 'NONE', *, *, #317, .T. ) ;
#11500 = CYLINDRICAL_SURFACE ( 'NONE', #8709, 2.800000000000003819 ) ;
#11501 = DIRECTION ( 'NONE',  ( 0.000000000000000000, 0.9195277725514489076, 0.3930250316539277144 ) ) ;
#11502 = FACE_OUTER_BOUND ( 'NONE', #1215, .T. ) ;
#11503 = DIRECTION ( 'NONE',  ( -1.000000000000000000, 1.010728034814421376E-30, 1.090846720500930387E-30 ) ) ;
#11504 = ORIENTED_EDGE ( 'NONE', *, *, #9650, .T. ) ;
#11505 = DIRECTION ( 'NONE',  ( 0.000000000000000000, 0.000000000000000000, 1.000000000000000000 ) ) ;
#11506 = VECTOR ( 'NONE', #1278, 1000.000000000000000 ) ;
#11507 = AXIS2_PLACEMENT_3D ( 'NONE', #7081, #2185, #2121 ) ;
#11508 = AXIS2_PLACEMENT_3D ( 'NONE', #6088, #11964, #9166 ) ;
#11509 = DIRECTION ( 'NONE',  ( 1.000000000000000000, -0.000000000000000000, -0.000000000000000000 ) ) ;
#11510 = ORIENTED_EDGE ( 'NONE', *, *, #9033, .T. ) ;
#11511 = ORIENTED_EDGE ( 'NONE', *, *, #11006, .F. ) ;
#11512 = LINE ( 'NONE', #10650, #8840 ) ;
#11513 = ORIENTED_EDGE ( 'NONE', *, *, #10351, .F. ) ;
#11514 = SHAPE_REPRESENTATION ( 'cover 2', ( #12422 ), #5765 ) ;
#11515 = ORIENTED_EDGE ( 'NONE', *, *, #8846, .F. ) ;
#11516 = CARTESIAN_POINT ( 'NONE',  ( 0.000000000000000000, -5.651611091574845425, 4.776954267060575354 ) ) ;
#11517 = AXIS2_PLACEMENT_3D ( 'NONE', #581, #1679, #11348 ) ;
#11518 = CARTESIAN_POINT ( 'NONE',  ( -37.15000000000005542, 2.632990618166567153E-16, 2.000000000000003553 ) ) ;
#11519 = AXIS2_PLACEMENT_3D ( 'NONE', #2812, #8715, #12593 ) ;
#11520 = ORIENTED_EDGE ( 'NONE', *, *, #12558, .F. ) ;
#11521 = CARTESIAN_POINT ( 'NONE',  ( 19.99999999999999645, 6.718789039999943924, 3.101269713516811688 ) ) ;
#11522 = CYLINDRICAL_SURFACE ( 'NONE', #2461, 4.000000000000000000 ) ;
#11523 = EDGE_LOOP ( 'NONE', ( #7118, #5583, #6569, #5423 ) ) ;
#11524 = AXIS2_PLACEMENT_3D ( 'NONE', #12160, #6414, #9049 ) ;
#11525 = DIRECTION ( 'NONE',  ( -1.000000000000000000, 1.006188713385347367E-17, 3.844790828812615713E-17 ) ) ;
#11526 = CARTESIAN_POINT ( 'NONE',  ( 19.99999999999997868, 7.100173756228451261, -2.085073771204482007 ) ) ;
#11527 = LINE ( 'NONE', #11885, #11632 ) ;
#11528 = CIRCLE ( 'NONE', #6588, 1.535500000000001863 ) ;
#11529 = AXIS2_PLACEMENT_3D ( 'NONE', #3121, #2211, #7926 ) ;
#11530 = CIRCLE ( 'NONE', #5141, 2.149999999999999023 ) ;
#11531 = EDGE_LOOP ( 'NONE', ( #10262, #6483, #21, #2892 ) ) ;
#11532 = VERTEX_POINT ( 'NONE', #11746 ) ;
#11533 = PLANE ( 'NONE',  #3161 ) ;
#11534 = DIRECTION ( 'NONE',  ( 0.000000000000000000, 2.135047315880774263E-19, -1.000000000000000222 ) ) ;
#11535 = ORIENTED_EDGE ( 'NONE', *, *, #10892, .F. ) ;
#11536 = CARTESIAN_POINT ( 'NONE',  ( 19.99999999999999645, 0.000000000000000000, 0.000000000000000000 ) ) ;
#11537 = AXIS2_PLACEMENT_3D ( 'NONE', #5700, #11574, #8595 ) ;
#11538 = CIRCLE ( 'NONE', #12154, 6.000000000000000888 ) ;
#11539 = VECTOR ( 'NONE', #1283, 1000.000000000000000 ) ;
#11540 = CARTESIAN_POINT ( 'NONE',  ( 9.714451465470119729E-14, 0.8865213383406691516, -1.535500000000002085 ) ) ;
#11541 = ADVANCED_FACE ( 'NONE', ( #5566 ), #8265, .T. ) ;
#11542 = PRODUCT_DEFINITION_SHAPE ( 'NONE', 'NONE',  #12750 ) ;
#11543 = EDGE_CURVE ( 'NONE', #3396, #2015, #4389, .T. ) ;
#11544 = ADVANCED_FACE ( 'NONE', ( #10825 ), #11024, .F. ) ;
#11545 = DIRECTION ( 'NONE',  ( -1.000000000000000000, 1.010728034814421376E-30, 1.090846720500930387E-30 ) ) ;
#11546 = CARTESIAN_POINT ( 'NONE',  ( 0.000000000000000000, 0.000000000000000000, 0.000000000000000000 ) ) ;
#11547 = VERTEX_POINT ( 'NONE', #5042 ) ;
#11548 = CARTESIAN_POINT ( 'NONE',  ( 0.000000000000000000, 0.000000000000000000, 0.000000000000000000 ) ) ;
#11549 = ORIENTED_EDGE ( 'NONE', *, *, #23, .F. ) ;
#11550 = CARTESIAN_POINT ( 'NONE',  ( -35.00000000000006395, -2.157041537713704155E-29, 2.168404344971033323E-15 ) ) ;
#11551 =( NAMED_UNIT ( * ) SI_UNIT ( $, .STERADIAN. ) SOLID_ANGLE_UNIT ( ) );
#11552 = FACE_OUTER_BOUND ( 'NONE', #6434, .T. ) ;
#11553 = DIRECTION ( 'NONE',  ( 0.000000000000000000, -1.000000000000000000, 0.000000000000000000 ) ) ;
#11554 = DIRECTION ( 'NONE',  ( 0.000000000000000000, 0.000000000000000000, -1.000000000000000000 ) ) ;
#11555 = CARTESIAN_POINT ( 'NONE',  ( 33.00000000000001421, 81.84122341717352356, -52.68198508464162444 ) ) ;
#11556 = DIRECTION ( 'NONE',  ( 0.000000000000000000, -1.000000000000000000, 0.000000000000000000 ) ) ;
#11557 = CARTESIAN_POINT ( 'NONE',  ( 9.999999999999998224, 1.528443194675510153, -7.240432404259457222 ) ) ;
#11558 = CARTESIAN_POINT ( 'NONE',  ( -31.74999999999995026, 0.000000000000000000, 3.499999999999982681 ) ) ;
#11559 = DIRECTION ( 'NONE',  ( 5.916456789157575403E-31, -1.000000000000000000, -1.177425296209239362E-30 ) ) ;
#11560 = ADVANCED_FACE ( 'NONE', ( #8957 ), #11876, .F. ) ;
#11561 = LINE ( 'NONE', #10575, #7437 ) ;
#11562 = EDGE_LOOP ( 'NONE', ( #4818, #5093, #9899, #6689 ) ) ;
#11563 = ORIENTED_EDGE ( 'NONE', *, *, #1356, .T. ) ;
#11564 = VERTEX_POINT ( 'NONE', #206 ) ;
#11565 = DIRECTION ( 'NONE',  ( 1.000000000000000000, 0.000000000000000000, -1.159061634649218351E-16 ) ) ;
#11566 = DIRECTION ( 'NONE',  ( -1.000000000000000000, 1.010728034814421376E-30, 1.090846720500930387E-30 ) ) ;
#11567 = CARTESIAN_POINT ( 'NONE',  ( 27.00000000000001066, 39.92642927056392210, -44.05727230799563898 ) ) ;
#11568 = EDGE_CURVE ( 'NONE', #4184, #7175, #9788, .T. ) ;
#11569 = CARTESIAN_POINT ( 'NONE',  ( 9.000000000000031974, -6.123233995736752477E-16, 17.85000000000003695 ) ) ;
#11570 = ORIENTED_EDGE ( 'NONE', *, *, #2597, .F. ) ;
#11571 = EDGE_CURVE ( 'NONE', #2818, #235, #6917, .T. ) ;
#11572 = DIRECTION ( 'NONE',  ( 0.000000000000000000, 0.000000000000000000, 1.000000000000000000 ) ) ;
#11573 = VECTOR ( 'NONE', #4263, 1000.000000000000000 ) ;
#11574 = DIRECTION ( 'NONE',  ( -1.000000000000000000, 1.010728034814421376E-30, 1.090846720500930387E-30 ) ) ;
#11575 = VERTEX_POINT ( 'NONE', #8051 ) ;
#11576 = VERTEX_POINT ( 'NONE', #3122 ) ;
#11577 = CARTESIAN_POINT ( 'NONE',  ( 19.99999999999999645, -4.518585619147920340, 5.860237538055056206 ) ) ;
#11578 = ORIENTED_EDGE ( 'NONE', *, *, #6057, .T. ) ;
#11579 = ORIENTED_EDGE ( 'NONE', *, *, #2999, .T. ) ;
#11580 = AXIS2_PLACEMENT_3D ( 'NONE', #9260, #3488, #10215 ) ;
#11581 = CARTESIAN_POINT ( 'NONE',  ( 19.99999999999999645, 2.649444137877595473, 6.020675595748703479 ) ) ;
#11582 = ORIENTED_EDGE ( 'NONE', *, *, #9891, .T. ) ;
#11583 = DIRECTION ( 'NONE',  ( 0.000000000000000000, 0.000000000000000000, -1.000000000000000000 ) ) ;
#11584 = FACE_OUTER_BOUND ( 'NONE', #8010, .T. ) ;
#11585 = ORIENTED_EDGE ( 'NONE', *, *, #6529, .F. ) ;
#11586 = DIRECTION ( 'NONE',  ( 1.000000000000000000, -1.010728034814421376E-30, -1.090846720500930387E-30 ) ) ;
#11587 = CARTESIAN_POINT ( 'NONE',  ( -15.00000000000000000, -20.00000000000000000, 9.850000000000033396 ) ) ;
#11588 = VECTOR ( 'NONE', #4330, 1000.000000000000000 ) ;
#11589 = AXIS2_PLACEMENT_3D ( 'NONE', #8808, #9887, #54 ) ;
#11590 = ADVANCED_FACE ( 'NONE', ( #19 ), #11939, .T. ) ;
#11591 = VERTEX_POINT ( 'NONE', #12002 ) ;
#11592 = ORIENTED_EDGE ( 'NONE', *, *, #2278, .F. ) ;
#11593 = CARTESIAN_POINT ( 'NONE',  ( 14.00000000000000000, -13.00000000000000000, 0.000000000000000000 ) ) ;
#11594 = CARTESIAN_POINT ( 'NONE',  ( 13.00000000000000711, -19.99999999999999645, -12.00000000000006928 ) ) ;
#11595 = ORIENTED_EDGE ( 'NONE', *, *, #10410, .F. ) ;
#11596 = DIRECTION ( 'NONE',  ( -1.000000000000000000, 1.010728034814421376E-30, 1.090846720500930387E-30 ) ) ;
#11597 = DIRECTION ( 'NONE',  ( 1.000000000000000000, -1.010728034814421376E-30, -1.090846720500930387E-30 ) ) ;
#11598 = CARTESIAN_POINT ( 'NONE',  ( 0.000000000000000000, 7.380072687735805381, 0.5427035320837054755 ) ) ;
#11599 = VECTOR ( 'NONE', #4462, 1000.000000000000000 ) ;
#11600 = FACE_OUTER_BOUND ( 'NONE', #6807, .T. ) ;
#11601 = ORIENTED_EDGE ( 'NONE', *, *, #3289, .T. ) ;
#11602 = CARTESIAN_POINT ( 'NONE',  ( -17.00000000000002842, -20.00000000000000000, 14.15000000000003055 ) ) ;
#11603 = VERTEX_POINT ( 'NONE', #2141 ) ;
#11604 = CARTESIAN_POINT ( 'NONE',  ( 14.00000000000000000, 44.64000000000000057, 3.999999999999993339 ) ) ;
#11605 = EDGE_CURVE ( 'NONE', #6292, #1053, #3000, .T. ) ;
#11606 = EDGE_CURVE ( 'NONE', #5369, #5504, #6637, .T. ) ;
#11607 = DIRECTION ( 'NONE',  ( -1.000000000000000000, 1.010728034814421376E-30, 1.090846720500930387E-30 ) ) ;
#11608 = CIRCLE ( 'NONE', #3988, 2.800000000000004263 ) ;
#11609 = DIRECTION ( 'NONE',  ( 0.000000000000000000, 0.000000000000000000, 1.000000000000000000 ) ) ;
#11610 = CARTESIAN_POINT ( 'NONE',  ( 19.99999999999997868, 6.544726022087254513, 0.6592800351837256878 ) ) ;
#11611 = DIRECTION ( 'NONE',  ( -3.260214209858707948E-30, -0.5000000000000012212, -0.8660254037844380415 ) ) ;
#11612 = CARTESIAN_POINT ( 'NONE',  ( 4.211140560182228043, -2.431303136016558231, -3.745885042887437510 ) ) ;
#11613 = CARTESIAN_POINT ( 'NONE',  ( 19.99999999999997868, -1.113123845672304491, -7.315801754025040182 ) ) ;
#11614 = AXIS2_PLACEMENT_3D ( 'NONE', #3452, #6140, #5365 ) ;
#11615 = CARTESIAN_POINT ( 'NONE',  ( 11.17157287525379772, -30.00000000000000000, -2.828427124746177856 ) ) ;
#11616 = DIRECTION ( 'NONE',  ( -0.000000000000000000, -1.000000000000000000, -0.000000000000000000 ) ) ;
#11617 = UNCERTAINTY_MEASURE_WITH_UNIT (LENGTH_MEASURE( 1.000000000000000082E-05 ), #12424, 'distance_accuracy_value', 'NONE');
#11618 = LINE ( 'NONE', #787, #4135 ) ;
#11619 = EDGE_CURVE ( 'NONE', #12630, #4356, #5933, .T. ) ;
#11620 = AXIS2_PLACEMENT_3D ( 'NONE', #1803, #10740, #8755 ) ;
#11621 = ORIENTED_EDGE ( 'NONE', *, *, #6655, .T. ) ;
#11622 = CIRCLE ( 'NONE', #300, 0.2000000000000000944 ) ;
#11623 = ORIENTED_EDGE ( 'NONE', *, *, #1228, .F. ) ;
#11624 = CARTESIAN_POINT ( 'NONE',  ( 19.99999999999999645, 7.164568425986759692, 1.851744925564481559 ) ) ;
#11625 = CARTESIAN_POINT ( 'NONE',  ( 4.000000000000000000, 0.000000000000000000, 0.000000000000000000 ) ) ;
#11626 = DIRECTION ( 'NONE',  ( -0.7071067811865445751, 0.000000000000000000, 0.7071067811865504593 ) ) ;
#11627 = DIRECTION ( 'NONE',  ( -1.000000000000000000, 0.000000000000000000, 0.000000000000000000 ) ) ;
#11628 = ORIENTED_EDGE ( 'NONE', *, *, #9441, .T. ) ;
#11629 = FACE_OUTER_BOUND ( 'NONE', #5772, .T. ) ;
#11630 = CARTESIAN_POINT ( 'NONE',  ( 14.00000000000000000, 44.64000000000000057, -5.000000000000000888 ) ) ;
#11631 = ORIENTED_EDGE ( 'NONE', *, *, #8723, .T. ) ;
#11632 = VECTOR ( 'NONE', #10903, 1000.000000000000000 ) ;
#11633 = VECTOR ( 'NONE', #6344, 1000.000000000000000 ) ;
#11634 = ORIENTED_EDGE ( 'NONE', *, *, #2184, .F. ) ;
#11635 = CARTESIAN_POINT ( 'NONE',  ( 2.500000000000035527, -3.163285252166775924E-15, -4.974600000000009459 ) ) ;
#11636 = VERTEX_POINT ( 'NONE', #1102 ) ;
#11637 = ORIENTED_EDGE ( 'NONE', *, *, #1159, .T. ) ;
#11638 = EDGE_CURVE ( 'NONE', #10601, #7844, #7032, .T. ) ;
#11639 = EDGE_CURVE ( 'NONE', #3527, #11393, #3190, .T. ) ;
#11640 = DIRECTION ( 'NONE',  ( -1.000000000000000000, 1.010728034814421376E-30, 1.090846720500930387E-30 ) ) ;
#11641 = VERTEX_POINT ( 'NONE', #1232 ) ;
#11642 = CARTESIAN_POINT ( 'NONE',  ( -17.00000000000002842, -20.00000000000000000, 14.15000000000003588 ) ) ;
#11643 = CARTESIAN_POINT ( 'NONE',  ( 19.99999999999999645, 6.018220532833773007, 2.453165835849278942 ) ) ;
#11644 = VERTEX_POINT ( 'NONE', #6064 ) ;
#11645 = CIRCLE ( 'NONE', #320, 2.800000000000002931 ) ;
#11646 = DIRECTION ( 'NONE',  ( -0.000000000000000000, -1.530455820933490821E-32, 1.000000000000000000 ) ) ;
#11647 = EDGE_CURVE ( 'NONE', #335, #6983, #5382, .T. ) ;
#11648 = DIRECTION ( 'NONE',  ( -1.000000000000000000, 1.010728034814421376E-30, 1.090846720500930387E-30 ) ) ;
#11649 = VERTEX_POINT ( 'NONE', #9084 ) ;
#11650 = ORIENTED_EDGE ( 'NONE', *, *, #12744, .F. ) ;
#11651 = ORIENTED_EDGE ( 'NONE', *, *, #3792, .T. ) ;
#11652 = AXIS2_PLACEMENT_3D ( 'NONE', #1066, #8083, #11969 ) ;
#11653 = CARTESIAN_POINT ( 'NONE',  ( 19.99999999999999645, -4.907279493584704610, -4.380262188593404105 ) ) ;
#11654 = CIRCLE ( 'NONE', #10405, 10.00000000000000178 ) ;
#11655 = DIRECTION ( 'NONE',  ( 1.764928971381541919E-16, -0.7878259692088108723, -0.6158979154374514264 ) ) ;
#11656 = VERTEX_POINT ( 'NONE', #3060 ) ;
#11657 = DIRECTION ( 'NONE',  ( -1.140150527077241873E-30, 0.000000000000000000, 1.000000000000000000 ) ) ;
#11658 = ORIENTED_EDGE ( 'NONE', *, *, #2359, .F. ) ;
#11659 = DIRECTION ( 'NONE',  ( 0.000000000000000000, 0.000000000000000000, 1.000000000000000000 ) ) ;
#11660 = VECTOR ( 'NONE', #11627, 1000.000000000000000 ) ;
#11661 = CARTESIAN_POINT ( 'NONE',  ( -4.211140560182161430, -2.431303136016561783, -3.745885042887451277 ) ) ;
#11662 = DIRECTION ( 'NONE',  ( -1.000000000000000000, 1.010728034814421376E-30, 1.090846720500930387E-30 ) ) ;
#11663 = VERTEX_POINT ( 'NONE', #8894 ) ;
#11664 = CARTESIAN_POINT ( 'NONE',  ( 4.024499207728844397, 2.323545700935675473, -3.572172305156859462 ) ) ;
#11665 = VERTEX_POINT ( 'NONE', #80 ) ;
#11666 = DIRECTION ( 'NONE',  ( -1.000000000000000000, 1.010728034814421376E-30, 1.090846720500930387E-30 ) ) ;
#11667 = PRODUCT_DEFINITION_FORMATION_WITH_SPECIFIED_SOURCE ( 'ANY', '', #4427, .NOT_KNOWN. ) ;
#11668 = SURFACE_STYLE_FILL_AREA ( #8705 ) ;
#11669 = CIRCLE ( 'NONE', #2417, 4.000000000000000000 ) ;
#11670 = AXIS2_PLACEMENT_3D ( 'NONE', #6531, #11489, #1430 ) ;
#11671 = DIRECTION ( 'NONE',  ( 1.238279320584846685E-16, -0.9554649393887560960, 0.2951046417778627751 ) ) ;
#11672 = CYLINDRICAL_SURFACE ( 'NONE', #42, 7.999999999999998224 ) ;
#11673 = CYLINDRICAL_SURFACE ( 'NONE', #11403, 2.149999999999992362 ) ;
#11674 = CARTESIAN_POINT ( 'NONE',  ( 27.00000000000001776, 48.04086878529346194, 39.26975893117280947 ) ) ;
#11675 = CARTESIAN_POINT ( 'NONE',  ( 1.393927851585494260, -4.043713361053535849, -3.526374918436848027 ) ) ;
#11676 = EDGE_CURVE ( 'NONE', #9287, #12081, #11356, .T. ) ;
#11677 = DIRECTION ( 'NONE',  ( -0.000000000000000000, -1.000000000000000000, -0.000000000000000000 ) ) ;
#11678 = CARTESIAN_POINT ( 'NONE',  ( 0.000000000000000000, 0.000000000000000000, 0.000000000000000000 ) ) ;
#11679 = AXIS2_PLACEMENT_3D ( 'NONE', #7067, #4164, #358 ) ;
#11680 = DIRECTION ( 'NONE',  ( 1.000000000000000000, 0.000000000000000000, 0.000000000000000000 ) ) ;
#11681 = DIRECTION ( 'NONE',  ( 0.000000000000000000, 0.000000000000000000, -1.000000000000000000 ) ) ;
#11682 = ORIENTED_EDGE ( 'NONE', *, *, #929, .F. ) ;
#11683 = EDGE_LOOP ( 'NONE', ( #10589, #8718, #10975, #1507 ) ) ;
#11684 = LINE ( 'NONE', #2879, #10971 ) ;
#11685 = CARTESIAN_POINT ( 'NONE',  ( 0.000000000000000000, -4.907279493584765895, 4.380262188593320616 ) ) ;
#11686 = CARTESIAN_POINT ( 'NONE',  ( 0.000000000000000000, -6.486618105788061861, -0.4009819817180140800 ) ) ;
#11687 = EDGE_LOOP ( 'NONE', ( #5506, #12108, #8857, #11191, #5596 ) ) ;
#11688 = EDGE_CURVE ( 'NONE', #303, #9408, #1686, .T. ) ;
#11689 = DIRECTION ( 'NONE',  ( 1.000000000000000000, 0.000000000000000000, 0.000000000000000000 ) ) ;
#11690 = ADVANCED_FACE ( 'NONE', ( #8118 ), #6855, .T. ) ;
#11691 = CARTESIAN_POINT ( 'NONE',  ( 0.000000000000000000, 0.000000000000000000, 0.000000000000000000 ) ) ;
#11692 = VERTEX_POINT ( 'NONE', #1944 ) ;
#11693 = ORIENTED_EDGE ( 'NONE', *, *, #7517, .T. ) ;
#11694 = FACE_OUTER_BOUND ( 'NONE', #9249, .T. ) ;
#11695 = VERTEX_POINT ( 'NONE', #395 ) ;
#11696 = ORIENTED_EDGE ( 'NONE', *, *, #11983, .T. ) ;
#11697 = DIRECTION ( 'NONE',  ( -9.614242282381069117E-31, -0.08963930890344097568, 0.9959742939952382912 ) ) ;
#11698 = VERTEX_POINT ( 'NONE', #8381 ) ;
#11699 = DIRECTION ( 'NONE',  ( -1.000000000000000000, -5.916456789157575403E-31, 1.577021341797099039E-16 ) ) ;
#11700 = DIRECTION ( 'NONE',  ( 0.000000000000000000, 1.000000000000000000, 0.000000000000000000 ) ) ;
#11701 = ORIENTED_EDGE ( 'NONE', *, *, #1864, .F. ) ;
#11702 = EDGE_CURVE ( 'NONE', #349, #9732, #2522, .T. ) ;
#11703 = DIRECTION ( 'NONE',  ( 0.000000000000000000, 0.000000000000000000, -1.000000000000000000 ) ) ;
#11704 = CARTESIAN_POINT ( 'NONE',  ( 2.000000000000001776, -0.8865213383406727043, 1.535500000000009191 ) ) ;
#11705 = AXIS2_PLACEMENT_3D ( 'NONE', #2901, #6818, #6940 ) ;
#11706 = EDGE_CURVE ( 'NONE', #8622, #8864, #9149, .T. ) ;
#11707 = EDGE_CURVE ( 'NONE', #937, #2489, #1552, .T. ) ;
#11708 = EDGE_LOOP ( 'NONE', ( #582, #2894, #2262, #11570 ) ) ;
#11709 = VERTEX_POINT ( 'NONE', #11088 ) ;
#11710 = VECTOR ( 'NONE', #2006, 1000.000000000000000 ) ;
#11711 = VECTOR ( 'NONE', #3799, 1000.000000000000000 ) ;
#11712 = EDGE_LOOP ( 'NONE', ( #1026, #5000, #7399, #10712, #10285, #7138, #11239, #7785 ) ) ;
#11713 = CIRCLE ( 'NONE', #6778, 5.384454397937118664 ) ;
#11714 = CARTESIAN_POINT ( 'NONE',  ( 19.99999999999999645, -6.310777386698718239, 1.552768423021305022 ) ) ;
#11715 = EDGE_CURVE ( 'NONE', #4507, #7155, #8877, .T. ) ;
#11716 = VECTOR ( 'NONE', #10784, 1000.000000000000000 ) ;
#11717 = VERTEX_POINT ( 'NONE', #3441 ) ;
#11718 = LINE ( 'NONE', #5850, #9828 ) ;
#11719 = VERTEX_POINT ( 'NONE', #7360 ) ;
#11720 = DIRECTION ( 'NONE',  ( -1.000000000000000000, 1.010728034814421376E-30, 1.090846720500930387E-30 ) ) ;
#11721 = AXIS2_PLACEMENT_3D ( 'NONE', #8174, #315, #441 ) ;
#11722 = VECTOR ( 'NONE', #7103, 1000.000000000000000 ) ;
#11723 = AXIS2_PLACEMENT_3D ( 'NONE', #1780, #2834, #8605 ) ;
#11724 = EDGE_CURVE ( 'NONE', #9949, #4174, #11283, .T. ) ;
#11725 = EDGE_CURVE ( 'NONE', #3477, #3794, #3351, .T. ) ;
#11726 = DIRECTION ( 'NONE',  ( -1.000000000000000000, -1.031065855027150586E-29, 2.218671295934095703E-30 ) ) ;
#11727 = DIRECTION ( 'NONE',  ( -1.000000000000000000, 1.010728034814421376E-30, 1.090846720500930387E-30 ) ) ;
#11728 = ORIENTED_EDGE ( 'NONE', *, *, #12198, .F. ) ;
#11729 = CARTESIAN_POINT ( 'NONE',  ( 19.99999999999997868, 4.772487208025196992, -4.411390579991299354 ) ) ;
#11730 = VERTEX_POINT ( 'NONE', #3257 ) ;
#11731 = DIRECTION ( 'NONE',  ( 0.000000000000000000, 0.000000000000000000, 1.000000000000000000 ) ) ;
#11732 = CIRCLE ( 'NONE', #1651, 2.149999999999985256 ) ;
#11733 = SHAPE_REPRESENTATION_RELATIONSHIP ( 'NONE' , 'NONE' ,  #2726, #1739 ) ;
#11734 = CIRCLE ( 'NONE', #6173, 4.000000000000000000 ) ;
#11735 = CARTESIAN_POINT ( 'NONE',  ( 0.000000000000000000, 30.00000000000000000, -9.999999999999998224 ) ) ;
#11736 = LINE ( 'NONE', #73, #883 ) ;
#11737 = EDGE_CURVE ( 'NONE', #1778, #10994, #5486, .T. ) ;
#11738 = LINE ( 'NONE', #7744, #3044 ) ;
#11739 = CARTESIAN_POINT ( 'NONE',  ( 2.805705207896072029, -3.226868319750169967, -3.503898532754375239 ) ) ;
#11740 = CARTESIAN_POINT ( 'NONE',  ( -3.999999999999994671, -2.309401076758511806, -0.4999999999999865663 ) ) ;
#11741 = STYLED_ITEM ( 'NONE', ( #8604 ), #11121 ) ;
#11742 = CIRCLE ( 'NONE', #3520, 7.400000000000009237 ) ;
#11743 = CARTESIAN_POINT ( 'NONE',  ( 19.99999999999997868, 4.596015818000145359, -4.705818469689468486 ) ) ;
#11744 = ADVANCED_FACE ( 'NONE', ( #6193 ), #525, .T. ) ;
#11745 = DIRECTION ( 'NONE',  ( 1.000000000000000000, 1.848892746611742259E-31, -1.154721252774410375E-34 ) ) ;
#11746 = CARTESIAN_POINT ( 'NONE',  ( 1.999999999999994893, 1.329782007511003838, -0.7677500000000010427 ) ) ;
#11747 = EDGE_CURVE ( 'NONE', #7883, #5688, #10105, .T. ) ;
#11748 = B_SPLINE_CURVE_WITH_KNOTS ( 'NONE', 3,
 ( #5254, #2498, #10325, #2238, #9296, #487 ),
 .UNSPECIFIED., .F., .F.,
 ( 4, 2, 4 ),
 ( 0.002452478801916361563, 0.003676905084148001344, 0.004901331366379641126 ),
 .UNSPECIFIED. ) ;
#11749 = EDGE_LOOP ( 'NONE', ( #9883, #1372, #6614, #5534 ) ) ;
#11750 = FACE_OUTER_BOUND ( 'NONE', #1983, .T. ) ;
#11751 = DIRECTION ( 'NONE',  ( 0.000000000000000000, 0.000000000000000000, 1.000000000000000000 ) ) ;
#11752 = DIRECTION ( 'NONE',  ( 1.000000000000000000, -1.010728034814421376E-30, -1.090846720500930387E-30 ) ) ;
#11753 = CARTESIAN_POINT ( 'NONE',  ( 11.00000000000001599, 19.99999999999999645, 12.00000000000003020 ) ) ;
#11754 = CARTESIAN_POINT ( 'NONE',  ( 19.99999999999997868, 6.018220532833812975, -2.453165835849195453 ) ) ;
#11755 = VERTEX_POINT ( 'NONE', #6257 ) ;
#11756 = DIRECTION ( 'NONE',  ( 1.000000000000000000, 1.849040895279789448E-31, -6.938893903907224680E-17 ) ) ;
#11757 = EDGE_CURVE ( 'NONE', #3985, #11478, #2314, .T. ) ;
#11758 = CYLINDRICAL_SURFACE ( 'NONE', #1932, 10.00000000000002309 ) ;
#11759 = AXIS2_PLACEMENT_3D ( 'NONE', #6666, #1631, #4789 ) ;
#11760 = FILL_AREA_STYLE_COLOUR ( '', #9052 ) ;
#11761 = ORIENTED_EDGE ( 'NONE', *, *, #1245, .F. ) ;
#11762 = ORIENTED_EDGE ( 'NONE', *, *, #9256, .F. ) ;
#11763 = DIRECTION ( 'NONE',  ( 1.000000000000000000, -1.010728034814421376E-30, -1.090846720500930387E-30 ) ) ;
#11764 = EDGE_LOOP ( 'NONE', ( #3798, #10846, #8852, #8357 ) ) ;
#11765 = VERTEX_POINT ( 'NONE', #585 ) ;
#11766 = APPLICATION_PROTOCOL_DEFINITION ( 'draft international standard', 'automotive_design', 1998, #5918 ) ;
#11767 = EDGE_CURVE ( 'NONE', #2160, #10485, #7423, .T. ) ;
#11768 = CARTESIAN_POINT ( 'NONE',  ( 0.000000000000000000, -1.773042676681341856, 3.469446951953614189E-15 ) ) ;
#11769 = ADVANCED_FACE ( 'NONE', ( #8186 ), #6388, .T. ) ;
#11770 = EDGE_LOOP ( 'NONE', ( #5537, #2038, #7513 ) ) ;
#11771 = VECTOR ( 'NONE', #10357, 1000.000000000000227 ) ;
#11772 = DIRECTION ( 'NONE',  ( 0.000000000000000000, -0.9195277725514543476, 0.3930250316539148359 ) ) ;
#11773 = ADVANCED_FACE ( 'NONE', ( #1357 ), #12129, .T. ) ;
#11774 = DIRECTION ( 'NONE',  ( 0.000000000000000000, 0.000000000000000000, -1.000000000000000000 ) ) ;
#11775 = AXIS2_PLACEMENT_3D ( 'NONE', #7297, #2402, #10164 ) ;
#11776 = VERTEX_POINT ( 'NONE', #5292 ) ;
#11777 = DIRECTION ( 'NONE',  ( 0.000000000000000000, 5.551115123125777155E-17, 1.000000000000000000 ) ) ;
#11778 = DIRECTION ( 'NONE',  ( -1.000000000000000000, 1.010728034814421376E-30, 1.090846720500930387E-30 ) ) ;
#11779 = VERTEX_POINT ( 'NONE', #6457 ) ;
#11780 = VERTEX_POINT ( 'NONE', #11156 ) ;
#11781 = CIRCLE ( 'NONE', #2949, 1.000000000000000888 ) ;
#11782 = ORIENTED_EDGE ( 'NONE', *, *, #5988, .F. ) ;
#11783 = CYLINDRICAL_SURFACE ( 'NONE', #1701, 2.149999999999992362 ) ;
#11784 = EDGE_CURVE ( 'NONE', #11388, #8069, #4327, .T. ) ;
#11785 = ORIENTED_EDGE ( 'NONE', *, *, #6490, .T. ) ;
#11786 = CARTESIAN_POINT ( 'NONE',  ( 2.687328764639645762, -3.067272167851298192, -0.05923475698271467305 ) ) ;
#11787 = ORIENTED_EDGE ( 'NONE', *, *, #2814, .F. ) ;
#11788 = AXIS2_PLACEMENT_3D ( 'NONE', #2010, #2215, #8259 ) ;
#11789 = AXIS2_PLACEMENT_3D ( 'NONE', #3614, #699, #4636 ) ;
#11790 = EDGE_CURVE ( 'NONE', #8854, #8657, #5998, .T. ) ;
#11791 = DIRECTION ( 'NONE',  ( 0.000000000000000000, 0.000000000000000000, -1.000000000000000000 ) ) ;
#11792 = EDGE_CURVE ( 'NONE', #509, #47, #8046, .T. ) ;
#11793 = DIRECTION ( 'NONE',  ( 1.000000000000000000, 1.031065855027150586E-29, 2.218671295934092550E-30 ) ) ;
#11794 = ORIENTED_EDGE ( 'NONE', *, *, #7391, .T. ) ;
#11795 = DIRECTION ( 'NONE',  ( 0.000000000000000000, 0.000000000000000000, 1.000000000000000000 ) ) ;
#11796 = PRODUCT_DEFINITION_CONTEXT ( 'detailed design', #2, 'design' ) ;
#11797 = AXIS2_PLACEMENT_3D ( 'NONE', #9290, #4547, #2617 ) ;
#11798 = ORIENTED_EDGE ( 'NONE', *, *, #1757, .F. ) ;
#11799 = DIRECTION ( 'NONE',  ( -1.000000000000000000, 1.010728034814421376E-30, 1.090846720500930387E-30 ) ) ;
#11800 = EDGE_CURVE ( 'NONE', #3356, #5846, #1808, .T. ) ;
#11801 = CARTESIAN_POINT ( 'NONE',  ( 0.000000000000000000, 3.238809497145205718, 5.634457741540171760 ) ) ;
#11802 = EDGE_CURVE ( 'NONE', #10901, #8587, #9284, .T. ) ;
#11803 = CARTESIAN_POINT ( 'NONE',  ( 3.469446951953614189E-14, -3.469446951953614189E-15, -4.974600000000009459 ) ) ;
#11804 = VECTOR ( 'NONE', #4981, 1000.000000000000000 ) ;
#11805 = DIRECTION ( 'NONE',  ( -1.000000000000000000, 6.162975822039154730E-33, 4.563833282352349791E-17 ) ) ;
#11806 = LINE ( 'NONE', #7164, #4469 ) ;
#11807 = CARTESIAN_POINT ( 'NONE',  ( 3.469446951953614189E-14, -3.469446951953614189E-15, -4.974600000000009459 ) ) ;
#11808 = CARTESIAN_POINT ( 'NONE',  ( 4.200000000000001954, 2.694222958124178486E-16, 2.199999999999983746 ) ) ;
#11809 = CARTESIAN_POINT ( 'NONE',  ( 0.000000000000000000, 30.00000000000000000, 0.000000000000000000 ) ) ;
#11810 = CARTESIAN_POINT ( 'NONE',  ( -2.059999999999998721, 2.522772406243545965E-16, -0.3080913168122742518 ) ) ;
#11811 = AXIS2_PLACEMENT_3D ( 'NONE', #2253, #438, #8294 ) ;
#11812 = ORIENTED_EDGE ( 'NONE', *, *, #6965, .T. ) ;
#11813 = EDGE_LOOP ( 'NONE', ( #1834, #1719, #2339, #7710 ) ) ;
#11814 = DIRECTION ( 'NONE',  ( -1.000000000000000000, 1.010728034814421376E-30, 1.090846720500930387E-30 ) ) ;
#11815 = DIRECTION ( 'NONE',  ( 0.000000000000000000, -8.560894001270036306E-16, -1.000000000000000000 ) ) ;
#11816 = CARTESIAN_POINT ( 'NONE',  ( -14.99999999999999289, 30.00000000000000000, 25.00000000000007105 ) ) ;
#11817 = DIRECTION ( 'NONE',  ( -1.000000000000000000, 1.010728034814421376E-30, 1.090846720500930387E-30 ) ) ;
#11818 = VERTEX_POINT ( 'NONE', #11604 ) ;
#11819 = VECTOR ( 'NONE', #7434, 1000.000000000000000 ) ;
#11820 = EDGE_CURVE ( 'NONE', #8944, #1393, #3753, .T. ) ;
#11821 = LINE ( 'NONE', #5759, #7101 ) ;
#11822 = DIRECTION ( 'NONE',  ( 1.000000000000000000, 0.000000000000000000, 0.000000000000000000 ) ) ;
#11823 = PRODUCT_DEFINITION_SHAPE ( 'NONE', 'NONE',  #12759 ) ;
#11824 = LINE ( 'NONE', #6330, #396 ) ;
#11825 = VERTEX_POINT ( 'NONE', #713 ) ;
#11826 = EDGE_LOOP ( 'NONE', ( #4650, #11898, #11889, #9707 ) ) ;
#11827 = DIRECTION ( 'NONE',  ( -0.000000000000000000, -1.000000000000000000, -0.000000000000000000 ) ) ;
#11828 = VERTEX_POINT ( 'NONE', #839 ) ;
#11829 = AXIS2_PLACEMENT_3D ( 'NONE', #3317, #2398, #6189 ) ;
#11830 = ORIENTED_EDGE ( 'NONE', *, *, #11757, .F. ) ;
#11831 = SHAPE_DEFINITION_REPRESENTATION ( #10056, #10094 ) ;
#11832 = CIRCLE ( 'NONE', #712, 8.999999999999998224 ) ;
#11833 = DIRECTION ( 'NONE',  ( -1.848892746611746419E-31, -1.000000000000000000, 3.250006781153460502E-32 ) ) ;
#11834 = ORIENTED_EDGE ( 'NONE', *, *, #527, .T. ) ;
#11835 = DIRECTION ( 'NONE',  ( 0.000000000000000000, 1.000000000000000000, 0.000000000000000000 ) ) ;
#11836 = DIRECTION ( 'NONE',  ( 6.938893903907224680E-17, -1.040834085586079721E-15, 1.000000000000000000 ) ) ;
#11837 = ORIENTED_EDGE ( 'NONE', *, *, #12439, .T. ) ;
#11838 = CARTESIAN_POINT ( 'NONE',  ( 33.00000000000000000, 29.58047730022061472, -27.90351864933187898 ) ) ;
#11839 = DIRECTION ( 'NONE',  ( 1.000867273499157187E-29, 0.8660254037844380415, -0.5000000000000011102 ) ) ;
#11840 = VECTOR ( 'NONE', #11398, 1000.000000000000000 ) ;
#11841 = VECTOR ( 'NONE', #4613, 1000.000000000000000 ) ;
#11842 = EDGE_CURVE ( 'NONE', #8996, #2015, #1300, .T. ) ;
#11843 = ADVANCED_FACE ( 'NONE', ( #8703 ), #6773, .T. ) ;
#11844 = ORIENTED_EDGE ( 'NONE', *, *, #5796, .F. ) ;
#11845 = ORIENTED_EDGE ( 'NONE', *, *, #5959, .F. ) ;
#11846 = EDGE_LOOP ( 'NONE', ( #8632, #6943, #1902, #12291 ) ) ;
#11847 = CARTESIAN_POINT ( 'NONE',  ( 33.00000000000001421, 39.34792583643766761, -17.06347054209568270 ) ) ;
#11848 = VERTEX_POINT ( 'NONE', #2595 ) ;
#11849 = AXIS2_PLACEMENT_3D ( 'NONE', #6008, #1047, #7049 ) ;
#11850 = CARTESIAN_POINT ( 'NONE',  ( 2.855764796983347065, -2.970025579236429181, -0.09382832055446509167 ) ) ;
#11851 = ORIENTED_EDGE ( 'NONE', *, *, #3972, .T. ) ;
#11852 = CARTESIAN_POINT ( 'NONE',  ( 19.99999999999999645, -6.213893036447794671, -1.903820982021606989 ) ) ;
#11853 = EDGE_CURVE ( 'NONE', #5639, #3589, #1682, .T. ) ;
#11854 = DIRECTION ( 'NONE',  ( 0.000000000000000000, 0.000000000000000000, 1.000000000000000000 ) ) ;
#11855 = AXIS2_PLACEMENT_3D ( 'NONE', #11129, #115, #9060 ) ;
#11856 = VERTEX_POINT ( 'NONE', #7739 ) ;
#11857 = FACE_BOUND ( 'NONE', #9696, .T. ) ;
#11858 = ORIENTED_EDGE ( 'NONE', *, *, #3926, .F. ) ;
#11859 = PLANE ( 'NONE',  #8473 ) ;
#11860 =( NAMED_UNIT ( * ) PLANE_ANGLE_UNIT ( ) SI_UNIT ( $, .RADIAN. ) );
#11861 = PLANE ( 'NONE',  #821 ) ;
#11862 = CIRCLE ( 'NONE', #5080, 7.400000000000009237 ) ;
#11863 = FACE_OUTER_BOUND ( 'NONE', #7124, .T. ) ;
#11864 = AXIS2_PLACEMENT_3D ( 'NONE', #12028, #3279, #2303 ) ;
#11865 = CARTESIAN_POINT ( 'NONE',  ( 0.000000000000000000, -0.8865213383406761460, -1.535499999999995202 ) ) ;
#11866 = CARTESIAN_POINT ( 'NONE',  ( 19.99999999999999645, 0.000000000000000000, 0.000000000000000000 ) ) ;
#11867 = EDGE_CURVE ( 'NONE', #1279, #9645, #3947, .T. ) ;
#11868 = DIRECTION ( 'NONE',  ( -0.000000000000000000, -1.000000000000000000, -0.000000000000000000 ) ) ;
#11869 = EDGE_CURVE ( 'NONE', #3731, #5073, #8572, .T. ) ;
#11870 = DIRECTION ( 'NONE',  ( -1.140150527077241873E-30, 0.000000000000000000, 1.000000000000000000 ) ) ;
#11871 = AXIS2_PLACEMENT_3D ( 'NONE', #10487, #7473, #4578 ) ;
#11872 = EDGE_CURVE ( 'NONE', #10545, #8798, #8636, .T. ) ;
#11873 = FACE_OUTER_BOUND ( 'NONE', #3919, .T. ) ;
#11874 = AXIS2_PLACEMENT_3D ( 'NONE', #1365, #9399, #8511 ) ;
#11875 = AXIS2_PLACEMENT_3D ( 'NONE', #3130, #7045, #5110 ) ;
#11876 = CYLINDRICAL_SURFACE ( 'NONE', #3551, 2.149999999999999023 ) ;
#11877 = EDGE_CURVE ( 'NONE', #529, #10242, #10301, .T. ) ;
#11878 = EDGE_LOOP ( 'NONE', ( #8976, #5893, #2817, #4365 ) ) ;
#11879 = VERTEX_POINT ( 'NONE', #12451 ) ;
#11880 = CARTESIAN_POINT ( 'NONE',  ( 0.000000000000000000, 1.773042676681338303, 0.000000000000000000 ) ) ;
#11881 = FACE_OUTER_BOUND ( 'NONE', #2622, .T. ) ;
#11882 = DIRECTION ( 'NONE',  ( 0.000000000000000000, -0.3513748240813304724, -0.9362348706397417564 ) ) ;
#11883 = EDGE_LOOP ( 'NONE', ( #617, #1016, #9599, #5188 ) ) ;
#11884 = DIRECTION ( 'NONE',  ( -0.000000000000000000, -1.000000000000000000, -0.000000000000000000 ) ) ;
#11885 = CARTESIAN_POINT ( 'NONE',  ( 2.000000000000001776, 0.8865213383406622683, -1.535499999999995202 ) ) ;
#11886 = DIRECTION ( 'NONE',  ( 0.000000000000000000, 0.6579387259397138088, -0.7530714660036099684 ) ) ;
#11887 = ORIENTED_EDGE ( 'NONE', *, *, #9638, .T. ) ;
#11888 = B_SPLINE_CURVE_WITH_KNOTS ( 'NONE', 3,
 ( #10766, #9792, #7693, #25, #9666, #11625 ),
 .UNSPECIFIED., .F., .F.,
 ( 4, 2, 4 ),
 ( 0.003358874760055554493, 0.004541967308452099852, 0.005725059856848646080 ),
 .UNSPECIFIED. ) ;
#11889 = ORIENTED_EDGE ( 'NONE', *, *, #7782, .F. ) ;
#11890 = DIRECTION ( 'NONE',  ( 0.000000000000000000, 0.7227948638273881121, 0.6910626489868684219 ) ) ;
#11891 = ORIENTED_EDGE ( 'NONE', *, *, #11903, .F. ) ;
#11892 = ORIENTED_EDGE ( 'NONE', *, *, #11411, .T. ) ;
#11893 = APPLICATION_PROTOCOL_DEFINITION ( 'draft international standard', 'automotive_design', 1998, #409 ) ;
#11894 = CARTESIAN_POINT ( 'NONE',  ( 40.00000000000000711, 9.907988025913239127, -23.58742161290648554 ) ) ;
#11895 = ORIENTED_EDGE ( 'NONE', *, *, #2979, .F. ) ;
#11896 = FACE_OUTER_BOUND ( 'NONE', #10002, .T. ) ;
#11897 = DIRECTION ( 'NONE',  ( -1.000000000000000000, 0.000000000000000000, 0.000000000000000000 ) ) ;
#11898 = ORIENTED_EDGE ( 'NONE', *, *, #5869, .T. ) ;
#11899 = LINE ( 'NONE', #423, #10837 ) ;
#11900 = DIRECTION ( 'NONE',  ( 1.000000000000000000, 1.081682119347366197E-16, -6.938893903907228378E-17 ) ) ;
#11901 = CIRCLE ( 'NONE', #7407, 2.149999999999999023 ) ;
#11902 = ORIENTED_EDGE ( 'NONE', *, *, #11647, .F. ) ;
#11903 = EDGE_CURVE ( 'NONE', #1526, #7064, #2799, .T. ) ;
#11904 = VERTEX_POINT ( 'NONE', #12639 ) ;
#11905 = VERTEX_POINT ( 'NONE', #3810 ) ;
#11906 = DIRECTION ( 'NONE',  ( -2.126226658603505316E-31, 0.7818314824680310249, -0.6234898018587319291 ) ) ;
#11907 = LINE ( 'NONE', #4236, #7335 ) ;
#11908 = EDGE_LOOP ( 'NONE', ( #11436, #3092, #158, #399, #4478, #29 ) ) ;
#11909 = CARTESIAN_POINT ( 'NONE',  ( 40.00000000000000711, 8.524480291341571814, -16.78569157243880738 ) ) ;
#11910 = AXIS2_PLACEMENT_3D ( 'NONE', #11753, #9793, #1109 ) ;
#11911 = ORIENTED_EDGE ( 'NONE', *, *, #4728, .T. ) ;
#11912 = CARTESIAN_POINT ( 'NONE',  ( 40.00000000000006395, -2.499999999999997335, -20.00000000000000000 ) ) ;
#11913 = DIRECTION ( 'NONE',  ( -1.000000000000000000, 1.010728034814421376E-30, 1.090846720500930387E-30 ) ) ;
#11914 = AXIS2_PLACEMENT_3D ( 'NONE', #11678, #4785, #11870 ) ;
#11915 = AXIS2_PLACEMENT_3D ( 'NONE', #2574, #6628, #2509 ) ;
#11916 = CARTESIAN_POINT ( 'NONE',  ( 0.000000000000000000, 5.280167904461778861, -3.922743398397307679 ) ) ;
#11917 = ORIENTED_EDGE ( 'NONE', *, *, #3070, .T. ) ;
#11918 = AXIS2_PLACEMENT_3D ( 'NONE', #686, #8675, #9367 ) ;
#11919 = DIRECTION ( 'NONE',  ( 0.000000000000000000, 0.000000000000000000, 1.000000000000000000 ) ) ;
#11920 = VERTEX_POINT ( 'NONE', #7607 ) ;
#11921 = CARTESIAN_POINT ( 'NONE',  ( -45.00000000000001421, 19.99999999999999645, 2.000000000000007994 ) ) ;
#11922 = EDGE_CURVE ( 'NONE', #4963, #8313, #5798, .T. ) ;
#11923 = CARTESIAN_POINT ( 'NONE',  ( -15.00000000000000000, 30.00000000000000000, 3.000000000000029754 ) ) ;
#11924 = EDGE_CURVE ( 'NONE', #11959, #10196, #6652, .T. ) ;
#11925 = AXIS2_PLACEMENT_3D ( 'NONE', #9972, #9014, #10037 ) ;
#11926 = EDGE_CURVE ( 'NONE', #3630, #8559, #6845, .T. ) ;
#11927 = VECTOR ( 'NONE', #595, 1000.000000000000114 ) ;
#11928 = AXIS2_PLACEMENT_3D ( 'NONE', #9106, #5962, #8856 ) ;
#11929 = DIRECTION ( 'NONE',  ( 0.000000000000000000, 0.000000000000000000, 1.000000000000000000 ) ) ;
#11930 = CARTESIAN_POINT ( 'NONE',  ( -2.805705207896076914, 3.226868319750153535, -3.503898532754382344 ) ) ;
#11931 = AXIS2_PLACEMENT_3D ( 'NONE', #2857, #11720, #1863 ) ;
#11932 = CARTESIAN_POINT ( 'NONE',  ( 9.000000000000031974, -3.490243377569940777E-16, 22.15000000000003055 ) ) ;
#11933 = FACE_OUTER_BOUND ( 'NONE', #12114, .T. ) ;
#11934 = DIRECTION ( 'NONE',  ( -1.000000000000000000, 1.010728034814421376E-30, 1.090846720500930387E-30 ) ) ;
#11935 = LINE ( 'NONE', #6916, #12144 ) ;
#11936 = AXIS2_PLACEMENT_3D ( 'NONE', #4246, #3174, #2258 ) ;
#11937 = CIRCLE ( 'NONE', #8225, 2.800000000000004263 ) ;
#11938 = AXIS2_PLACEMENT_3D ( 'NONE', #5162, #7096, #9201 ) ;
#11939 = CYLINDRICAL_SURFACE ( 'NONE', #4575, 2.800000000000003819 ) ;
#11940 = VERTEX_POINT ( 'NONE', #2863 ) ;
#11941 = CARTESIAN_POINT ( 'NONE',  ( 19.99999999999999645, 0.3649881613860001539, 6.567714405409708078 ) ) ;
#11942 = FACE_OUTER_BOUND ( 'NONE', #1235, .T. ) ;
#11943 = PRESENTATION_LAYER_ASSIGNMENT (  '', '', ( #3519 ) ) ;
#11944 = CIRCLE ( 'NONE', #8649, 2.800000000000002931 ) ;
#11945 = FACE_OUTER_BOUND ( 'NONE', #6669, .T. ) ;
#11946 = DIRECTION ( 'NONE',  ( 0.000000000000000000, -0.5000000000000011102, -0.8660254037844379305 ) ) ;
#11947 = CIRCLE ( 'NONE', #7589, 6.499000000000008548 ) ;
#11948 = CARTESIAN_POINT ( 'NONE',  ( 19.99999999999999645, 0.000000000000000000, 0.000000000000000000 ) ) ;
#11949 = ORIENTED_EDGE ( 'NONE', *, *, #5186, .F. ) ;
#11950 = CARTESIAN_POINT ( 'NONE',  ( 9.000000000000035527, -19.99999999999999645, 12.00000000000003553 ) ) ;
#11951 = CARTESIAN_POINT ( 'NONE',  ( 2.886521338340684917, 0.000000000000000000, 1.387778780781445676E-14 ) ) ;
#11952 = ADVANCED_FACE ( 'NONE', ( #7481 ), #4708, .F. ) ;
#11953 = DIRECTION ( 'NONE',  ( -1.000000000000000000, 1.010728034814421376E-30, 1.090846720500930387E-30 ) ) ;
#11954 = ORIENTED_EDGE ( 'NONE', *, *, #4136, .F. ) ;
#11955 = ORIENTED_EDGE ( 'NONE', *, *, #11639, .F. ) ;
#11956 = DIRECTION ( 'NONE',  ( -1.140150527077241873E-30, 0.000000000000000000, 1.000000000000000000 ) ) ;
#11957 = VERTEX_POINT ( 'NONE', #6521 ) ;
#11958 = MECHANICAL_DESIGN_GEOMETRIC_PRESENTATION_REPRESENTATION (  '', ( #7628 ), #6190 ) ;
#11959 = VERTEX_POINT ( 'NONE', #12704 ) ;
#11960 = SHAPE_DEFINITION_REPRESENTATION ( #8112, #891 ) ;
#11961 = DIRECTION ( 'NONE',  ( -1.000000000000000000, 1.010728034814421376E-30, 1.090846720500930387E-30 ) ) ;
#11962 = ORIENTED_EDGE ( 'NONE', *, *, #1226, .T. ) ;
#11963 = EDGE_CURVE ( 'NONE', #568, #4499, #6429, .T. ) ;
#11964 = DIRECTION ( 'NONE',  ( -1.000000000000000000, 1.010728034814421376E-30, 1.090846720500930387E-30 ) ) ;
#11965 = ADVANCED_FACE ( 'NONE', ( #9773 ), #11859, .T. ) ;
#11966 = CARTESIAN_POINT ( 'NONE',  ( 19.99999999999999645, 0.000000000000000000, 0.000000000000000000 ) ) ;
#11967 = ORIENTED_EDGE ( 'NONE', *, *, #8367, .T. ) ;
#11968 = DIRECTION ( 'NONE',  ( -1.000000000000000000, 1.587729746749930812E-17, 7.204735498949985729E-17 ) ) ;
#11969 = DIRECTION ( 'NONE',  ( 0.000000000000000000, 0.2660368455666687337, 0.9639628606958550172 ) ) ;
#11970 = FACE_BOUND ( 'NONE', #4075, .T. ) ;
#11971 = AXIS2_PLACEMENT_3D ( 'NONE', #7373, #11298, #3332 ) ;
#11972 = ORIENTED_EDGE ( 'NONE', *, *, #6391, .F. ) ;
#11973 = ORIENTED_EDGE ( 'NONE', *, *, #5470, .F. ) ;
#11974 = VERTEX_POINT ( 'NONE', #10942 ) ;
#11975 = ORIENTED_EDGE ( 'NONE', *, *, #1114, .T. ) ;
#11976 = AXIS2_PLACEMENT_3D ( 'NONE', #3313, #7228, #11929 ) ;
#11977 = CARTESIAN_POINT ( 'NONE',  ( 33.00000000000000711, 39.92642927056392210, -44.05727230799563898 ) ) ;
#11978 = DIRECTION ( 'NONE',  ( -6.938893903907224680E-17, 3.250006781153453386E-32, -1.000000000000000000 ) ) ;
#11979 = ORIENTED_EDGE ( 'NONE', *, *, #10041, .T. ) ;
#11980 = DIRECTION ( 'NONE',  ( 0.000000000000000000, 0.000000000000000000, -1.000000000000000000 ) ) ;
#11981 = ORIENTED_EDGE ( 'NONE', *, *, #5018, .T. ) ;
#11982 = DIRECTION ( 'NONE',  ( -1.000000000000000000, 1.010728034814421376E-30, 1.090846720500930387E-30 ) ) ;
#11983 = EDGE_CURVE ( 'NONE', #8669, #12227, #11781, .T. ) ;
#11984 = DIRECTION ( 'NONE',  ( -1.000000000000000000, 1.010728034814421376E-30, 1.090846720500930387E-30 ) ) ;
#11985 = DIRECTION ( 'NONE',  ( -1.000000000000000000, 1.010728034814421376E-30, 1.090846720500930387E-30 ) ) ;
#11986 = EDGE_LOOP ( 'NONE', ( #4821, #6006, #308 ) ) ;
#11987 = DIRECTION ( 'NONE',  ( 1.577021341797099039E-16, 1.177425296209237084E-30, 1.000000000000000000 ) ) ;
#11988 = ORIENTED_EDGE ( 'NONE', *, *, #59, .F. ) ;
#11989 = FACE_OUTER_BOUND ( 'NONE', #2050, .T. ) ;
#11990 = TOROIDAL_SURFACE ( 'NONE', #9094, 2.200000000000001066, 0.2000000000000000111 ) ;
#11991 = CARTESIAN_POINT ( 'NONE',  ( 0.000000000000000000, 7.164568425986778344, -1.851744925564384525 ) ) ;
#11992 = DIRECTION ( 'NONE',  ( 0.000000000000000000, 0.000000000000000000, 1.000000000000000000 ) ) ;
#11993 = FACE_OUTER_BOUND ( 'NONE', #11749, .T. ) ;
#11994 = DIRECTION ( 'NONE',  ( -1.000000000000000000, -1.081682119347366444E-16, 5.551115123125780237E-17 ) ) ;
#11995 = AXIS2_PLACEMENT_3D ( 'NONE', #4348, #11437, #10250 ) ;
#11996 = DIRECTION ( 'NONE',  ( -1.224646799147352714E-16, -1.177425296209236909E-30, -1.000000000000000000 ) ) ;
#11997 = AXIS2_PLACEMENT_3D ( 'NONE', #1748, #5867, #11609 ) ;
#11998 = ADVANCED_FACE ( 'NONE', ( #5094 ), #6905, .T. ) ;
#11999 = VECTOR ( 'NONE', #240, 1000.000000000000000 ) ;
#12000 = LINE ( 'NONE', #4847, #11722 ) ;
#12001 = EDGE_CURVE ( 'NONE', #41, #3305, #6961, .T. ) ;
#12002 = CARTESIAN_POINT ( 'NONE',  ( 40.00000000000000711, 8.163911011730666800, -17.95311239921186441 ) ) ;
#12003 = AXIS2_PLACEMENT_3D ( 'NONE', #9728, #2943, #8779 ) ;
#12004 = EDGE_LOOP ( 'NONE', ( #1784, #11887, #2111, #5706 ) ) ;
#12005 = LINE ( 'NONE', #1236, #5406 ) ;
#12006 = LINE ( 'NONE', #1041, #74 ) ;
#12007 = CARTESIAN_POINT ( 'NONE',  ( 19.99999999999997868, 2.918117354836732513, -5.807029542149833468 ) ) ;
#12008 = DIRECTION ( 'NONE',  ( -1.000000000000000000, 1.010728034814421376E-30, 1.090846720500930387E-30 ) ) ;
#12009 = ORIENTED_EDGE ( 'NONE', *, *, #4033, .F. ) ;
#12010 = DIRECTION ( 'NONE',  ( -1.140150527077241873E-30, 0.000000000000000000, 1.000000000000000000 ) ) ;
#12011 = B_SPLINE_CURVE_WITH_KNOTS ( 'NONE', 3,
 ( #76, #4129, #8047, #4973, #11082, #6969 ),
 .UNSPECIFIED., .F., .F.,
 ( 4, 2, 4 ),
 ( 0.002365888236228003323, 0.003551327329835090186, 0.004736766423442177049 ),
 .UNSPECIFIED. ) ;
#12012 = DIRECTION ( 'NONE',  ( 0.000000000000000000, -0.9195277725514543476, 0.3930250316539147248 ) ) ;
#12013 = FACE_OUTER_BOUND ( 'NONE', #11126, .T. ) ;
#12014 = CIRCLE ( 'NONE', #11811, 5.560781378645573980 ) ;
#12015 = EDGE_CURVE ( 'NONE', #9489, #7883, #8683, .T. ) ;
#12016 = ORIENTED_EDGE ( 'NONE', *, *, #11853, .F. ) ;
#12017 = FACE_OUTER_BOUND ( 'NONE', #5516, .T. ) ;
#12018 = ORIENTED_EDGE ( 'NONE', *, *, #11193, .T. ) ;
#12019 = ORIENTED_EDGE ( 'NONE', *, *, #2441, .T. ) ;
#12020 = SHAPE_DEFINITION_REPRESENTATION ( #4644, #8305 ) ;
#12021 = DIRECTION ( 'NONE',  ( 0.000000000000000000, -0.9989930665413151445, 0.04486483035050449486 ) ) ;
#12022 = ORIENTED_EDGE ( 'NONE', *, *, #10201, .T. ) ;
#12023 = AXIS2_PLACEMENT_3D ( 'NONE', #657, #4537, #10634 ) ;
#12024 = DIRECTION ( 'NONE',  ( -1.000000000000000000, -1.081682119347366444E-16, 5.551115123125780237E-17 ) ) ;
#12025 = FACE_OUTER_BOUND ( 'NONE', #9370, .T. ) ;
#12026 = ORIENTED_EDGE ( 'NONE', *, *, #8298, .T. ) ;
#12027 = AXIS2_PLACEMENT_3D ( 'NONE', #6692, #7889, #3851 ) ;
#12028 = CARTESIAN_POINT ( 'NONE',  ( 4.200000000000001954, 0.000000000000000000, -1.734723475976807094E-14 ) ) ;
#12029 = CARTESIAN_POINT ( 'NONE',  ( 14.00000000000000000, 30.00000000000000000, 0.000000000000000000 ) ) ;
#12030 = CARTESIAN_POINT ( 'NONE',  ( 0.000000000000000000, 30.00000000000000000, -7.999999999999998224 ) ) ;
#12031 = CARTESIAN_POINT ( 'NONE',  ( 0.02448733951238716428, 4.877042772274719162, -3.751161874094028903 ) ) ;
#12032 = VERTEX_POINT ( 'NONE', #5864 ) ;
#12033 = AXIS2_PLACEMENT_3D ( 'NONE', #4515, #9452, #643 ) ;
#12034 = EDGE_CURVE ( 'NONE', #2488, #12043, #2113, .T. ) ;
#12035 = CIRCLE ( 'NONE', #9137, 7.400000000000011902 ) ;
#12036 = ORIENTED_EDGE ( 'NONE', *, *, #9108, .F. ) ;
#12037 = ORIENTED_EDGE ( 'NONE', *, *, #6007, .T. ) ;
#12038 = ADVANCED_FACE ( 'NONE', ( #11989 ), #3050, .T. ) ;
#12039 = EDGE_LOOP ( 'NONE', ( #6541, #10142, #8719, #7436 ) ) ;
#12040 = CARTESIAN_POINT ( 'NONE',  ( 20.00000000000000000, 21.12780530657007461, -5.807015647486883481 ) ) ;
#12041 = PRODUCT ( 'BR-598', 'BR-598', '', ( #8793 ) ) ;
#12042 = CARTESIAN_POINT ( 'NONE',  ( -0.6810597143199018655, -4.461075778259501412, -3.598441714920685541 ) ) ;
#12043 = VERTEX_POINT ( 'NONE', #6052 ) ;
#12044 = ADVANCED_FACE ( 'NONE', ( #963 ), #192, .F. ) ;
#12045 = LINE ( 'NONE', #11909, #8650 ) ;
#12046 = ORIENTED_EDGE ( 'NONE', *, *, #824, .T. ) ;
#12047 = AXIS2_PLACEMENT_3D ( 'NONE', #8100, #5271, #12050 ) ;
#12048 = AXIS2_PLACEMENT_3D ( 'NONE', #1387, #5316, #12224 ) ;
#12049 = DIRECTION ( 'NONE',  ( -1.000000000000000000, 1.010728034814421376E-30, 1.090846720500930387E-30 ) ) ;
#12050 = DIRECTION ( 'NONE',  ( 0.000000000000000000, -1.000000000000000000, 0.000000000000000000 ) ) ;
#12051 = CARTESIAN_POINT ( 'NONE',  ( 2.000000000000001776, 0.000000000000000000, 0.000000000000000000 ) ) ;
#12052 = ORIENTED_EDGE ( 'NONE', *, *, #10578, .T. ) ;
#12053 = DIRECTION ( 'NONE',  ( 0.000000000000000000, 0.000000000000000000, 1.000000000000000000 ) ) ;
#12054 = EDGE_LOOP ( 'NONE', ( #6492, #6960, #8224, #393, #5256 ) ) ;
#12055 = AXIS2_PLACEMENT_3D ( 'NONE', #9467, #3509, #4599 ) ;
#12056 = DIRECTION ( 'NONE',  ( -0.000000000000000000, -0.000000000000000000, -1.000000000000000000 ) ) ;
#12057 =( NAMED_UNIT ( * ) SI_UNIT ( $, .STERADIAN. ) SOLID_ANGLE_UNIT ( ) );
#12058 = LINE ( 'NONE', #9074, #11539 ) ;
#12059 = CARTESIAN_POINT ( 'NONE',  ( 19.99999999999999645, -4.357840574720558635, -4.821434073522041786 ) ) ;
#12060 = DIRECTION ( 'NONE',  ( 0.000000000000000000, -0.9510565162951500895, -0.3090169943749582759 ) ) ;
#12061 = FACE_OUTER_BOUND ( 'NONE', #7298, .T. ) ;
#12062 = CARTESIAN_POINT ( 'NONE',  ( 19.99999999999997868, 5.200656487704349296, -5.264330166022921809 ) ) ;
#12063 = DIRECTION ( 'NONE',  ( 0.000000000000000000, 0.000000000000000000, -1.000000000000000000 ) ) ;
#12064 =( NAMED_UNIT ( * ) SI_UNIT ( $, .STERADIAN. ) SOLID_ANGLE_UNIT ( ) );
#12065 = CIRCLE ( 'NONE', #7751, 2.800000000000002931 ) ;
#12066 = MECHANICAL_DESIGN_GEOMETRIC_PRESENTATION_REPRESENTATION (  '', ( #4240 ), #6717 ) ;
#12067 = VERTEX_POINT ( 'NONE', #3179 ) ;
#12068 = DIRECTION ( 'NONE',  ( 0.000000000000000000, 0.000000000000000000, 1.000000000000000000 ) ) ;
#12069 = ADVANCED_FACE ( 'NONE', ( #1027 ), #10746, .T. ) ;
#12070 = CARTESIAN_POINT ( 'NONE',  ( 9.999999999999998224, -4.707829255731169837, -5.709320773864598131 ) ) ;
#12071 = CARTESIAN_POINT ( 'NONE',  ( 14.00000000000000000, 30.00000000000000000, 0.000000000000000000 ) ) ;
#12072 = CARTESIAN_POINT ( 'NONE',  ( 11.00000000000003020, 30.00000000000000000, -7.347880794884148332E-16 ) ) ;
#12073 = ORIENTED_EDGE ( 'NONE', *, *, #5075, .F. ) ;
#12074 = DIRECTION ( 'NONE',  ( -1.000000000000000000, 1.010728034814421376E-30, 1.090846720500930387E-30 ) ) ;
#12075 = CIRCLE ( 'NONE', #1575, 6.000000000000000888 ) ;
#12076 = FACE_OUTER_BOUND ( 'NONE', #7329, .T. ) ;
#12077 = AXIS2_PLACEMENT_3D ( 'NONE', #10455, #6672, #11501 ) ;
#12078 =( NAMED_UNIT ( * ) PLANE_ANGLE_UNIT ( ) SI_UNIT ( $, .RADIAN. ) );
#12079 = ORIENTED_EDGE ( 'NONE', *, *, #5231, .F. ) ;
#12080 = DIRECTION ( 'NONE',  ( 1.000000000000000000, 1.081682119347366197E-16, -6.938893903907228378E-17 ) ) ;
#12081 = VERTEX_POINT ( 'NONE', #6 ) ;
#12082 = ORIENTED_EDGE ( 'NONE', *, *, #154, .F. ) ;
#12083 = EDGE_CURVE ( 'NONE', #2021, #6979, #10747, .T. ) ;
#12084 = CARTESIAN_POINT ( 'NONE',  ( 19.99999999999997868, -3.178467454237100309, -5.758943784352606343 ) ) ;
#12085 = ORIENTED_EDGE ( 'NONE', *, *, #8845, .T. ) ;
#12086 = CIRCLE ( 'NONE', #5290, 2.800000000000003819 ) ;
#12087 = DIRECTION ( 'NONE',  ( -1.000000000000000000, 1.010728034814421376E-30, 1.090846720500930387E-30 ) ) ;
#12088 = VECTOR ( 'NONE', #3053, 1000.000000000000000 ) ;
#12089 = EDGE_CURVE ( 'NONE', #2015, #11692, #4901, .T. ) ;
#12090 = CARTESIAN_POINT ( 'NONE',  ( 19.99999999999997868, 1.395418990828298567, -6.428133065596409068 ) ) ;
#12091 = EDGE_CURVE ( 'NONE', #4994, #1632, #1091, .T. ) ;
#12092 = VERTEX_POINT ( 'NONE', #11921 ) ;
#12093 = LINE ( 'NONE', #293, #5490 ) ;
#12095 = EDGE_CURVE ( 'NONE', #9218, #2245, #12607, .T. ) ;
#12094 = DIRECTION ( 'NONE',  ( -1.000000000000000000, 1.010728034814421376E-30, 1.090846720500930387E-30 ) ) ;
#12096 = DIRECTION ( 'NONE',  ( 1.000000000000000000, -0.000000000000000000, -6.938893903907228378E-17 ) ) ;
#12097 = CARTESIAN_POINT ( 'NONE',  ( 6.000000000000000000, 49.63999999999998636, -9.000000000000001776 ) ) ;
#12098 = ORIENTED_EDGE ( 'NONE', *, *, #2349, .T. ) ;
#12099 = VERTEX_POINT ( 'NONE', #10027 ) ;
#12100 = CIRCLE ( 'NONE', #11679, 6.000000000000000888 ) ;
#12101 = ORIENTED_EDGE ( 'NONE', *, *, #9824, .F. ) ;
#12102 = EDGE_LOOP ( 'NONE', ( #6372, #10450, #5734 ) ) ;
#12103 = DIRECTION ( 'NONE',  ( -1.000000000000000000, 1.010728034814421376E-30, 1.090846720500930387E-30 ) ) ;
#12104 = CARTESIAN_POINT ( 'NONE',  ( -2.836893136758698031, -3.208949435745759970, -3.505054077164898807 ) ) ;
#12105 = ORIENTED_EDGE ( 'NONE', *, *, #8453, .F. ) ;
#12106 = APPLICATION_CONTEXT ( 'automotive_design' ) ;
#12107 = LINE ( 'NONE', #11197, #10899 ) ;
#12108 = ORIENTED_EDGE ( 'NONE', *, *, #7899, .T. ) ;
#12109 = B_SPLINE_CURVE_WITH_KNOTS ( 'NONE', 3,
 ( #8018, #10184, #1380, #5310, #4347, #9746, #12485, #5833 ),
 .UNSPECIFIED., .F., .F.,
 ( 4, 2, 2, 4 ),
 ( 2.465131517396146612E-07, 0.001183067374689870379, 0.001774477805458936960, 0.002365888236228003323 ),
 .UNSPECIFIED. ) ;
#12110 = CARTESIAN_POINT ( 'NONE',  ( 19.99999999999997868, 0.3649881613860929686, -6.567714405409704526 ) ) ;
#12111 = FACE_OUTER_BOUND ( 'NONE', #3663, .T. ) ;
#12112 = CARTESIAN_POINT ( 'NONE',  ( 4.200000000000001954, 0.000000000000000000, 0.000000000000000000 ) ) ;
#12113 = ADVANCED_FACE ( 'NONE', ( #3111 ), #1219, .T. ) ;
#12114 = EDGE_LOOP ( 'NONE', ( #604, #6079, #3193, #298 ) ) ;
#12115 = FACE_BOUND ( 'NONE', #2466, .T. ) ;
#12116 = ORIENTED_EDGE ( 'NONE', *, *, #11213, .T. ) ;
#12117 = CARTESIAN_POINT ( 'NONE',  ( 40.00000000000000711, 16.67945018363952414, -6.690790236289299919 ) ) ;
#12118 = AXIS2_PLACEMENT_3D ( 'NONE', #11685, #983, #8901 ) ;
#12119 = SHAPE_REPRESENTATION_RELATIONSHIP ( 'NONE' , 'NONE' ,  #9199, #10947 ) ;
#12120 = CARTESIAN_POINT ( 'NONE',  ( 19.99999999999997868, 2.180689217871956131, -6.122221454264557217 ) ) ;
#12121 = ADVANCED_FACE ( 'NONE', ( #10812 ), #7915, .T. ) ;
#12122 = DIRECTION ( 'NONE',  ( -1.000000000000000000, 0.000000000000000000, 0.000000000000000000 ) ) ;
#12123 = EDGE_CURVE ( 'NONE', #2378, #4490, #5194, .T. ) ;
#12124 = VECTOR ( 'NONE', #7703, 1000.000000000000000 ) ;
#12125 = CARTESIAN_POINT ( 'NONE',  ( 14.00000000000000000, -13.00000000000000000, 0.000000000000000000 ) ) ;
#12126 = CARTESIAN_POINT ( 'NONE',  ( 9.999999999999998224, 5.200656487704351960, -5.264330166022921809 ) ) ;
#12127 = DIRECTION ( 'NONE',  ( -1.000000000000000000, 1.010728034814421376E-30, 1.090846720500930387E-30 ) ) ;
#12128 = DIRECTION ( 'NONE',  ( 0.000000000000000000, 0.9554649393887557629, -0.2951046417778634412 ) ) ;
#12129 = CYLINDRICAL_SURFACE ( 'NONE', #1885, 6.000000000000000000 ) ;
#12130 = CIRCLE ( 'NONE', #5336, 7.400000000000011902 ) ;
#12131 = AXIS2_PLACEMENT_3D ( 'NONE', #9309, #498, #4430 ) ;
#12133 = COLOUR_RGB ( '', 0.31764706, 0.68627451, 0.89019608) ;
#12132 =( NAMED_UNIT ( * ) SI_UNIT ( $, .STERADIAN. ) SOLID_ANGLE_UNIT ( ) );
#12134 = EDGE_CURVE ( 'NONE', #8459, #4118, #6181, .T. ) ;
#12135 = AXIS2_PLACEMENT_3D ( 'NONE', #10003, #1134, #12696 ) ;
#12136 = VERTEX_POINT ( 'NONE', #5404 ) ;
#12137 = CARTESIAN_POINT ( 'NONE',  ( 20.00000000000006750, 2.499999999999997780, -20.00000000000000000 ) ) ;
#12138 = CARTESIAN_POINT ( 'NONE',  ( 19.99999999999999645, -3.730839900301496925, -5.321450426182552818 ) ) ;
#12139 = CARTESIAN_POINT ( 'NONE',  ( -4.211405944401390933, -2.460460786169392566, -3.751298493805505174 ) ) ;
#12140 = DIRECTION ( 'NONE',  ( 0.000000000000000000, -0.5000000000000012212, -0.8660254037844380415 ) ) ;
#12141 = ADVANCED_FACE ( 'NONE', ( #7158 ), #11144, .F. ) ;
#12142 = DIRECTION ( 'NONE',  ( 1.000000000000000000, 0.000000000000000000, 0.000000000000000000 ) ) ;
#12143 = VECTOR ( 'NONE', #5983, 1000.000000000000000 ) ;
#12144 = VECTOR ( 'NONE', #10822, 1000.000000000000000 ) ;
#12145 = VECTOR ( 'NONE', #11833, 1000.000000000000000 ) ;
#12146 = DIRECTION ( 'NONE',  ( -4.930380657631325535E-31, -1.000000000000000000, -1.177425296209239362E-30 ) ) ;
#12147 = EDGE_CURVE ( 'NONE', #2245, #2575, #3306, .T. ) ;
#12148 = CARTESIAN_POINT ( 'NONE',  ( 20.00000000000000000, 0.000000000000000000, 0.000000000000000000 ) ) ;
#12149 = ORIENTED_EDGE ( 'NONE', *, *, #8671, .T. ) ;
#12150 = CARTESIAN_POINT ( 'NONE',  ( 3.999999999999996447, 3.500000000000003109, 0.000000000000000000 ) ) ;
#12151 = EDGE_LOOP ( 'NONE', ( #1254, #8411, #2226, #1715 ) ) ;
#12152 = ORIENTED_EDGE ( 'NONE', *, *, #9954, .T. ) ;
#12153 = STYLED_ITEM ( 'NONE', ( #12476 ), #9919 ) ;
#12154 = AXIS2_PLACEMENT_3D ( 'NONE', #4185, #4249, #12357 ) ;
#12155 = ORIENTED_EDGE ( 'NONE', *, *, #8915, .T. ) ;
#12156 = CIRCLE ( 'NONE', #1029, 2.800000000000002931 ) ;
#12157 = CARTESIAN_POINT ( 'NONE',  ( 19.99999999999997868, 4.494880553659097444, -4.802513683199186367 ) ) ;
#12158 = CARTESIAN_POINT ( 'NONE',  ( 0.000000000000000000, 0.000000000000000000, 0.000000000000000000 ) ) ;
#12159 = CARTESIAN_POINT ( 'NONE',  ( 0.000000000000000000, -0.9522442067291368994, 6.508557431545707317 ) ) ;
#12160 = CARTESIAN_POINT ( 'NONE',  ( 19.99999999999999645, -5.682309657208315379, -3.313524683562055984 ) ) ;
#12161 = EDGE_CURVE ( 'NONE', #9207, #4167, #4583, .T. ) ;
#12162 = DIRECTION ( 'NONE',  ( -1.000000000000000000, 1.006188713385347367E-17, 3.844790828812615713E-17 ) ) ;
#12163 = CARTESIAN_POINT ( 'NONE',  ( -0.5276280594147285674, 4.314175951381911567, -3.320322319201698846 ) ) ;
#12164 = PRESENTATION_LAYER_ASSIGNMENT (  '', '', ( #4332 ) ) ;
#12165 = DIRECTION ( 'NONE',  ( 1.000000000000000000, 5.916456789157575403E-31, -1.577021341797098546E-16 ) ) ;
#12166 = EDGE_LOOP ( 'NONE', ( #8087, #4475, #9295, #6703, #1844 ) ) ;
#12167 = ORIENTED_EDGE ( 'NONE', *, *, #1630, .F. ) ;
#12168 = EDGE_CURVE ( 'NONE', #701, #3305, #3760, .T. ) ;
#12169 = ORIENTED_EDGE ( 'NONE', *, *, #11842, .T. ) ;
#12170 = EDGE_CURVE ( 'NONE', #1632, #9207, #1072, .T. ) ;
#12171 = VERTEX_POINT ( 'NONE', #11075 ) ;
#12172 = CARTESIAN_POINT ( 'NONE',  ( 19.99999999999999645, 1.834336845376711933, 6.234758161925244124 ) ) ;
#12173 = CARTESIAN_POINT ( 'NONE',  ( 19.99999999999997868, -7.301715115245777099, 1.202063382601481489 ) ) ;
#12174 = VERTEX_POINT ( 'NONE', #8304 ) ;
#12175 = CARTESIAN_POINT ( 'NONE',  ( -10.00000000000000178, 0.000000000000000000, 0.000000000000000000 ) ) ;
#12176 = ORIENTED_EDGE ( 'NONE', *, *, #12742, .F. ) ;
#12177 = CARTESIAN_POINT ( 'NONE',  ( -2.345747346278108658, 3.264484291692490547, -0.01223254789873496305 ) ) ;
#12178 = CARTESIAN_POINT ( 'NONE',  ( -3.511755186886760693, 2.826662030176358087, -3.597382984111575421 ) ) ;
#12179 = CARTESIAN_POINT ( 'NONE',  ( 19.99999999999999645, -6.577476285968329783, 0.06996125000489905599 ) ) ;
#12180 = DIRECTION ( 'NONE',  ( 0.000000000000000000, 0.000000000000000000, 1.000000000000000000 ) ) ;
#12181 = ORIENTED_EDGE ( 'NONE', *, *, #8794, .F. ) ;
#12182 = AXIS2_PLACEMENT_3D ( 'NONE', #9404, #411, #10243 ) ;
#12183 = EDGE_CURVE ( 'NONE', #3728, #11717, #6307, .T. ) ;
#12184 = ORIENTED_EDGE ( 'NONE', *, *, #12486, .F. ) ;
#12185 = CARTESIAN_POINT ( 'NONE',  ( 0.000000000000000000, -12.99999999999999822, 0.000000000000000000 ) ) ;
#12186 = CARTESIAN_POINT ( 'NONE',  ( -3.999999999999992450, 1.563622288139195682, -0.2253451193528239471 ) ) ;
#12187 = DIRECTION ( 'NONE',  ( 0.000000000000000000, 0.8805955318567392220, -0.4738686624729964159 ) ) ;
#12188 = EDGE_CURVE ( 'NONE', #4291, #5068, #7224, .T. ) ;
#12189 = AXIS2_PLACEMENT_3D ( 'NONE', #2213, #9975, #6130 ) ;
#12190 = DIRECTION ( 'NONE',  ( -4.683861624749750588E-31, -0.4338837391175658365, 0.9009688679024154823 ) ) ;
#12191 = PLANE ( 'NONE',  #3196 ) ;
#12192 = FACE_OUTER_BOUND ( 'NONE', #11446, .T. ) ;
#12193 = EDGE_LOOP ( 'NONE', ( #12073, #7540, #7961, #4826 ) ) ;
#12194 = CARTESIAN_POINT ( 'NONE',  ( 27.00000000000001421, 39.34792583643766761, -14.56347054209569158 ) ) ;
#12195 = ADVANCED_FACE ( 'NONE', ( #6244 ), #12310, .T. ) ;
#12196 = DIRECTION ( 'NONE',  ( -0.000000000000000000, -1.000000000000000000, -0.000000000000000000 ) ) ;
#12197 = AXIS2_PLACEMENT_3D ( 'NONE', #2198, #2929, #9835 ) ;
#12198 = EDGE_CURVE ( 'NONE', #11765, #7155, #10151, .T. ) ;
#12199 = SURFACE_SIDE_STYLE ('',( #8188 ) ) ;
#12200 = EDGE_CURVE ( 'NONE', #11320, #5702, #9492, .T. ) ;
#12201 = ORIENTED_EDGE ( 'NONE', *, *, #6754, .F. ) ;
#12202 = LINE ( 'NONE', #1106, #3766 ) ;
#12203 = EDGE_CURVE ( 'NONE', #4276, #3082, #1895, .T. ) ;
#12204 = CARTESIAN_POINT ( 'NONE',  ( 19.99999999999999645, -6.310777386698697811, -1.552768423021409161 ) ) ;
#12205 = CARTESIAN_POINT ( 'NONE',  ( 19.99999999999997868, 1.531833341630222112, -6.396997380212695816 ) ) ;
#12206 = CARTESIAN_POINT ( 'NONE',  ( 2.000000000000001776, 1.329782007511007169, 0.7677499999999976010 ) ) ;
#12207 = AXIS2_PLACEMENT_3D ( 'NONE', #4138, #8055, #6197 ) ;
#12208 = CARTESIAN_POINT ( 'NONE',  ( 19.99999999999997868, 6.359534927042319374, -1.339147681075104845 ) ) ;
#12209 = VECTOR ( 'NONE', #9948, 1000.000000000000000 ) ;
#12210 = DIRECTION ( 'NONE',  ( 0.000000000000000000, 0.000000000000000000, 1.000000000000000000 ) ) ;
#12211 =( NAMED_UNIT ( * ) SI_UNIT ( $, .STERADIAN. ) SOLID_ANGLE_UNIT ( ) );
#12212 = ORIENTED_EDGE ( 'NONE', *, *, #9176, .T. ) ;
#12213 = FACE_OUTER_BOUND ( 'NONE', #223, .T. ) ;
#12214 = VERTEX_POINT ( 'NONE', #381 ) ;
#12215 = AXIS2_PLACEMENT_3D ( 'NONE', #10722, #1908, #5647 ) ;
#12216 = ORIENTED_EDGE ( 'NONE', *, *, #4455, .F. ) ;
#12217 = EDGE_LOOP ( 'NONE', ( #4081, #9946, #9862, #12565, #7764, #6950, #9643, #9432, #10579, #5456, #2700, #12278, #950, #8554, #8060, #5606, #9160, #11059, #2689, #9804, #7073, #4879 ) ) ;
#12218 = CARTESIAN_POINT ( 'NONE',  ( 2.000000000000001776, -1.773042676681348739, 1.387778780781445676E-14 ) ) ;
#12219 = CARTESIAN_POINT ( 'NONE',  ( -35.00000000000006395, -2.157041537713704155E-29, 2.000000000000002220 ) ) ;
#12220 = LINE ( 'NONE', #3402, #1980 ) ;
#12221 = DIRECTION ( 'NONE',  ( -1.238279320584846685E-16, 0.9554649393887558739, -0.2951046417778634412 ) ) ;
#12222 = DIRECTION ( 'NONE',  ( 0.000000000000000000, 5.551115123125776539E-17, 1.000000000000000000 ) ) ;
#12223 = ORIENTED_EDGE ( 'NONE', *, *, #304, .F. ) ;
#12224 = DIRECTION ( 'NONE',  ( 0.000000000000000000, 0.9749279121818227312, 0.2225209339563182509 ) ) ;
#12225 = VECTOR ( 'NONE', #8260, 1000.000000000000000 ) ;
#12226 = DIRECTION ( 'NONE',  ( -1.000000000000000000, -2.206481006425900381E-16, 8.674603474570137221E-17 ) ) ;
#12227 = VERTEX_POINT ( 'NONE', #4312 ) ;
#12228 = VERTEX_POINT ( 'NONE', #1408 ) ;
#12229 = ORIENTED_EDGE ( 'NONE', *, *, #12561, .F. ) ;
#12230 = ORIENTED_EDGE ( 'NONE', *, *, #7898, .F. ) ;
#12231 = DIRECTION ( 'NONE',  ( -1.000000000000000000, 1.010728034814421376E-30, 1.090846720500930387E-30 ) ) ;
#12232 = CIRCLE ( 'NONE', #6678, 2.149999999999999023 ) ;
#12233 = FILL_AREA_STYLE_COLOUR ( '', #8355 ) ;
#12234 = ORIENTED_EDGE ( 'NONE', *, *, #11877, .F. ) ;
#12235 = DIRECTION ( 'NONE',  ( -1.000000000000000000, -1.081682119347366197E-16, 6.938893903907228378E-17 ) ) ;
#12236 = ORIENTED_EDGE ( 'NONE', *, *, #8133, .F. ) ;
#12237 = LINE ( 'NONE', #3422, #1104 ) ;
#12238 = EDGE_CURVE ( 'NONE', #2941, #4489, #9085, .T. ) ;
#12239 = DIRECTION ( 'NONE',  ( 1.000000000000000000, -1.010728034814421376E-30, -1.090846720500930387E-30 ) ) ;
#12240 = DIRECTION ( 'NONE',  ( -1.000000000000000000, 0.000000000000000000, 0.000000000000000000 ) ) ;
#12241 = CARTESIAN_POINT ( 'NONE',  ( 20.00000000000000000, 11.34118543499637077, -24.03007857557328464 ) ) ;
#12242 = ORIENTED_EDGE ( 'NONE', *, *, #3740, .F. ) ;
#12243 = ORIENTED_EDGE ( 'NONE', *, *, #8008, .T. ) ;
#12244 = DIRECTION ( 'NONE',  ( -1.000000000000000000, 1.010728034814421376E-30, 1.090846720500930387E-30 ) ) ;
#12245 = VECTOR ( 'NONE', #7789, 1000.000000000000000 ) ;
#12246 = AXIS2_PLACEMENT_3D ( 'NONE', #6696, #5774, #9563 ) ;
#12247 = DIRECTION ( 'NONE',  ( 1.000000000000000000, 1.849040895279789667E-31, -6.938893903907224680E-17 ) ) ;
#12248 = DIRECTION ( 'NONE',  ( -1.224646799147352714E-16, -1.177425296209236909E-30, -1.000000000000000000 ) ) ;
#12249 = PRODUCT_DEFINITION_SHAPE ( 'NONE', 'NONE',  #9002 ) ;
#12250 = EDGE_CURVE ( 'NONE', #11665, #8458, #8105, .T. ) ;
#12251 = PRODUCT_DEFINITION ( 'UNKNOWN', '', #2845, #11203 ) ;
#12252 = CARTESIAN_POINT ( 'NONE',  ( 9.000000000000017764, 19.99999999999999645, 12.00000000000003020 ) ) ;
#12253 = DIRECTION ( 'NONE',  ( 1.000000000000000000, 0.000000000000000000, 0.000000000000000000 ) ) ;
#12254 = AXIS2_PLACEMENT_3D ( 'NONE', #9051, #2433, #8343 ) ;
#12255 = CYLINDRICAL_SURFACE ( 'NONE', #11925, 2.800000000000003819 ) ;
#12256 = ORIENTED_EDGE ( 'NONE', *, *, #12250, .T. ) ;
#12257 = FACE_OUTER_BOUND ( 'NONE', #4743, .T. ) ;
#12258 = CARTESIAN_POINT ( 'NONE',  ( 19.99999999999999645, 0.000000000000000000, 0.000000000000000000 ) ) ;
#12259 = SURFACE_STYLE_USAGE ( .BOTH. , #12199 ) ;
#12260 = ORIENTED_EDGE ( 'NONE', *, *, #2838, .F. ) ;
#12261 = VECTOR ( 'NONE', #277, 1000.000000000000114 ) ;
#12262 = DIRECTION ( 'NONE',  ( 0.000000000000000000, 0.000000000000000000, 1.000000000000000000 ) ) ;
#12263 = CARTESIAN_POINT ( 'NONE',  ( 19.99999999999997868, -3.426907987218776874, -5.522074125465566752 ) ) ;
#12264 = CARTESIAN_POINT ( 'NONE',  ( 2.000000000000007105, 3.464101615137750390, 6.938893903907228378E-15 ) ) ;
#12265 = EDGE_CURVE ( 'NONE', #11190, #4291, #11341, .T. ) ;
#12266 = CARTESIAN_POINT ( 'NONE',  ( 0.000000000000000000, -0.1095571986795065844, 6.498076501567022767 ) ) ;
#12267 = DIRECTION ( 'NONE',  ( 0.000000000000000000, 0.000000000000000000, 1.000000000000000000 ) ) ;
#12268 = ADVANCED_FACE ( 'NONE', ( #4444 ), #6445, .T. ) ;
#12269 = DIRECTION ( 'NONE',  ( -1.000000000000000000, 1.010728034814421376E-30, 1.090846720500930387E-30 ) ) ;
#12270 = DIRECTION ( 'NONE',  ( -3.260214209858707948E-30, -0.5000000000000012212, -0.8660254037844380415 ) ) ;
#12271 = APPLICATION_CONTEXT ( 'automotive_design' ) ;
#12272 = ORIENTED_EDGE ( 'NONE', *, *, #8874, .T. ) ;
#12273 = ADVANCED_FACE ( 'NONE', ( #7529 ), #6700, .T. ) ;
#12274 = VECTOR ( 'NONE', #11978, 1000.000000000000000 ) ;
#12275 = CYLINDRICAL_SURFACE ( 'NONE', #11971, 2.000000000000000888 ) ;
#12276 = ORIENTED_EDGE ( 'NONE', *, *, #6449, .T. ) ;
#12277 = ORIENTED_EDGE ( 'NONE', *, *, #9458, .F. ) ;
#12278 = ORIENTED_EDGE ( 'NONE', *, *, #7312, .T. ) ;
#12279 = ORIENTED_EDGE ( 'NONE', *, *, #12598, .T. ) ;
#12280 = CARTESIAN_POINT ( 'NONE',  ( 0.000000000000000000, -6.459281472512942379, -1.243290685169453402 ) ) ;
#12281 = DIRECTION ( 'NONE',  ( -1.000000000000000000, 1.010728034814421376E-30, 1.090846720500930387E-30 ) ) ;
#12282 = CARTESIAN_POINT ( 'NONE',  ( 11.00000000000003375, 12.50000000000000000, 5.000000000000004441 ) ) ;
#12283 = AXIS2_PLACEMENT_3D ( 'NONE', #7996, #2152, #9922 ) ;
#12284 = ADVANCED_FACE ( 'NONE', ( #10546 ), #2583, .F. ) ;
#12285 = CARTESIAN_POINT ( 'NONE',  ( 0.000000000000000000, 5.025702764809159895, -5.431603052487340655 ) ) ;
#12286 = ORIENTED_EDGE ( 'NONE', *, *, #5832, .T. ) ;
#12287 = CIRCLE ( 'NONE', #5274, 3.500000000000000000 ) ;
#12288 = EDGE_CURVE ( 'NONE', #9180, #3594, #11470, .T. ) ;
#12289 = DIRECTION ( 'NONE',  ( 0.000000000000000000, -6.695352868347750602E-17, 1.000000000000000000 ) ) ;
#12290 = CARTESIAN_POINT ( 'NONE',  ( 27.00000000000000000, 44.40501137213340144, -30.19113521482024964 ) ) ;
#12291 = ORIENTED_EDGE ( 'NONE', *, *, #4561, .T. ) ;
#12292 = ORIENTED_EDGE ( 'NONE', *, *, #12666, .F. ) ;
#12293 = ORIENTED_EDGE ( 'NONE', *, *, #7200, .T. ) ;
#12294 = ORIENTED_EDGE ( 'NONE', *, *, #10033, .F. ) ;
#12295 = CIRCLE ( 'NONE', #9998, 2.800000000000003819 ) ;
#12296 = DIRECTION ( 'NONE',  ( -0.000000000000000000, -1.000000000000000000, -0.000000000000000000 ) ) ;
#12297 = CIRCLE ( 'NONE', #6736, 2.800000000000002931 ) ;
#12298 = VERTEX_POINT ( 'NONE', #6509 ) ;
#12299 = LINE ( 'NONE', #7397, #6578 ) ;
#12300 = ORIENTED_EDGE ( 'NONE', *, *, #3201, .F. ) ;
#12301 = CARTESIAN_POINT ( 'NONE',  ( 0.6507732100473474501, -4.243078065514793273, -0.2236248678334946949 ) ) ;
#12302 = LINE ( 'NONE', #12371, #3608 ) ;
#12303 = EDGE_CURVE ( 'NONE', #2371, #9180, #7050, .T. ) ;
#12304 = DIRECTION ( 'NONE',  ( 0.000000000000000000, 0.000000000000000000, 1.000000000000000000 ) ) ;
#12305 = PRODUCT_DEFINITION_CONTEXT ( 'detailed design', #1067, 'design' ) ;
#12306 = CARTESIAN_POINT ( 'NONE',  ( 15.00000000000003375, 12.50000000000000000, -4.000000000000000000 ) ) ;
#12307 = EDGE_CURVE ( 'NONE', #9645, #9939, #9568, .T. ) ;
#12308 = ORIENTED_EDGE ( 'NONE', *, *, #10823, .T. ) ;
#12309 = EDGE_LOOP ( 'NONE', ( #10120, #3143, #4231, #6018 ) ) ;
#12310 = PLANE ( 'NONE',  #11580 ) ;
#12311 = CARTESIAN_POINT ( 'NONE',  ( 15.00000000000003375, -12.49999999999999645, -6.000000000000000000 ) ) ;
#12312 = FACE_OUTER_BOUND ( 'NONE', #12498, .T. ) ;
#12313 = DIRECTION ( 'NONE',  ( 0.000000000000000000, 0.000000000000000000, -1.000000000000000000 ) ) ;
#12314 = DIRECTION ( 'NONE',  ( -1.000000000000000000, 1.010728034814421376E-30, 1.090846720500930387E-30 ) ) ;
#12315 = DIRECTION ( 'NONE',  ( -0.7071067811865445751, 0.000000000000000000, 0.7071067811865504593 ) ) ;
#12316 = EDGE_LOOP ( 'NONE', ( #5076, #2422, #226, #3141 ) ) ;
#12317 = CIRCLE ( 'NONE', #11524, 2.800000000000003375 ) ;
#12318 = CARTESIAN_POINT ( 'NONE',  ( 19.99999999999999645, 0.000000000000000000, 0.000000000000000000 ) ) ;
#12319 = CARTESIAN_POINT ( 'NONE',  ( 0.000000000000000000, 6.321830586517956263, -1.817291089601262621 ) ) ;
#12320 = EDGE_CURVE ( 'NONE', #3023, #444, #2537, .T. ) ;
#12321 = EDGE_CURVE ( 'NONE', #6259, #10923, #9505, .T. ) ;
#12322 = ADVANCED_FACE ( 'NONE', ( #8431 ), #7659, .T. ) ;
#12323 = FILL_AREA_STYLE_COLOUR ( '', #1035 ) ;
#12324 = EDGE_CURVE ( 'NONE', #11175, #1427, #10952, .T. ) ;
#12325 = CARTESIAN_POINT ( 'NONE',  ( 0.000000000000000000, -2.385831757338500836, -6.045230171438896072 ) ) ;
#12326 = ORIENTED_EDGE ( 'NONE', *, *, #6020, .T. ) ;
#12327 = FACE_OUTER_BOUND ( 'NONE', #10423, .T. ) ;
#12328 = DIRECTION ( 'NONE',  ( -1.000000000000000000, -1.031065855027150586E-29, 2.218671295934095703E-30 ) ) ;
#12329 = AXIS2_PLACEMENT_3D ( 'NONE', #10521, #8661, #2821 ) ;
#12330 = DIRECTION ( 'NONE',  ( -1.000000000000000000, 1.010728034814421376E-30, 1.090846720500930387E-30 ) ) ;
#12331 = DIRECTION ( 'NONE',  ( 1.000000000000000000, -1.010728034814421376E-30, -1.090846720500930387E-30 ) ) ;
#12332 = DIRECTION ( 'NONE',  ( 0.000000000000000000, 0.000000000000000000, -1.000000000000000000 ) ) ;
#12333 = CARTESIAN_POINT ( 'NONE',  ( 0.000000000000000000, -7.301715115245786869, 1.202063382601481489 ) ) ;
#12334 = AXIS2_PLACEMENT_3D ( 'NONE', #1291, #8049, #3187 ) ;
#12335 = CIRCLE ( 'NONE', #4714, 6.000000000000000888 ) ;
#12336 = STYLED_ITEM ( 'NONE', ( #12403 ), #10231 ) ;
#12337 = DIRECTION ( 'NONE',  ( -1.000000000000000000, 1.010728034814421376E-30, 1.090846720500930387E-30 ) ) ;
#12338 = ORIENTED_EDGE ( 'NONE', *, *, #4483, .T. ) ;
#12339 = VECTOR ( 'NONE', #6877, 1000.000000000000000 ) ;
#12340 = ADVANCED_FACE ( 'NONE', ( #3674 ), #1733, .T. ) ;
#12341 =( BOUNDED_SURFACE ( )  B_SPLINE_SURFACE ( 3, 2, ( 
 ( #394, #6192, #458 ),
 ( #10038, #9330, #4390 ),
 ( #7167, #6385, #10104 ),
 ( #10297, #524, #11350 ),
 ( #1486, #4454, #2534 ),
 ( #10432, #3806, #6585 ) ),
 .UNSPECIFIED., .F., .F., .T. ) 
 B_SPLINE_SURFACE_WITH_KNOTS ( ( 4, 2, 4 ),
 ( 3, 3 ),
 ( 0.02032853247518126225, 0.02278863295364821212, 0.02524873343211516200 ),
 ( 0.000000000000000000, 1.000000000000000000 ),
 .UNSPECIFIED. ) 
 GEOMETRIC_REPRESENTATION_ITEM ( )  RATIONAL_B_SPLINE_SURFACE ( (
 ( 1.000000000000000000, 0.8047781615896835161, 1.000000000000000000),
 ( 1.000000000000000000, 0.8123767586289977194, 1.000000000000000000),
 ( 1.000000000000000000, 0.8190662415563441101, 1.000000000000000000),
 ( 1.000000000000000000, 0.8192361015669979984, 1.000000000000000000),
 ( 1.000000000000000000, 0.8126135807103183062, 1.000000000000000000),
 ( 1.000000000000000000, 0.8047712338318581127, 1.000000000000000000) ) ) 
 REPRESENTATION_ITEM ( '' )  SURFACE ( )  );
#12342 = ORIENTED_EDGE ( 'NONE', *, *, #481, .T. ) ;
#12343 = ORIENTED_EDGE ( 'NONE', *, *, #1942, .T. ) ;
#12344 = DIRECTION ( 'NONE',  ( -1.000000000000000000, -5.916456789157575403E-31, 1.577021341797098793E-16 ) ) ;
#12345 = AXIS2_PLACEMENT_3D ( 'NONE', #123, #10741, #7790 ) ;
#12346 = CARTESIAN_POINT ( 'NONE',  ( 19.99999999999999645, -5.774092856145700559, -2.982759240804946810 ) ) ;
#12347 = DIRECTION ( 'NONE',  ( -1.238279320584846685E-16, 0.9554649393887558739, -0.2951046417778634412 ) ) ;
#12348 = MECHANICAL_DESIGN_GEOMETRIC_PRESENTATION_REPRESENTATION (  '', ( #6367 ), #1013 ) ;
#12349 = VECTOR ( 'NONE', #3274, 1000.000000000000000 ) ;
#12350 = DIRECTION ( 'NONE',  ( -1.848892746611746419E-31, -1.000000000000000000, 3.250006781153460502E-32 ) ) ;
#12351 = EDGE_LOOP ( 'NONE', ( #10013, #3534, #4223, #5601, #4024 ) ) ;
#12352 = EDGE_CURVE ( 'NONE', #7997, #10168, #9910, .T. ) ;
#12353 = DIRECTION ( 'NONE',  ( 0.000000000000000000, 1.000000000000000000, 0.000000000000000000 ) ) ;
#12354 = DIRECTION ( 'NONE',  ( 1.000000000000000000, 0.000000000000000000, -1.159061634649218351E-16 ) ) ;
#12355 = ORIENTED_EDGE ( 'NONE', *, *, #4147, .T. ) ;
#12356 = ORIENTED_EDGE ( 'NONE', *, *, #714, .T. ) ;
#12357 = DIRECTION ( 'NONE',  ( 0.000000000000000000, 0.000000000000000000, 1.000000000000000000 ) ) ;
#12358 = ORIENTED_EDGE ( 'NONE', *, *, #5694, .T. ) ;
#12359 = VECTOR ( 'NONE', #11337, 1000.000000000000000 ) ;
#12360 = ORIENTED_EDGE ( 'NONE', *, *, #414, .T. ) ;
#12361 = AXIS2_PLACEMENT_3D ( 'NONE', #1681, #7541, #7670 ) ;
#12362 = AXIS2_PLACEMENT_3D ( 'NONE', #6447, #1605, #5476 ) ;
#12363 = ADVANCED_FACE ( 'NONE', ( #8685 ), #11533, .F. ) ;
#12364 =( NAMED_UNIT ( * ) SI_UNIT ( $, .STERADIAN. ) SOLID_ANGLE_UNIT ( ) );
#12365 = PRESENTATION_STYLE_ASSIGNMENT (( #8415 ) ) ;
#12366 = ORIENTED_EDGE ( 'NONE', *, *, #2864, .T. ) ;
#12367 = CARTESIAN_POINT ( 'NONE',  ( 40.00000000000000000, 39.34792583643766051, -17.06347054209567915 ) ) ;
#12368 = CARTESIAN_POINT ( 'NONE',  ( 0.000000000000000000, 0.3649881613859949914, 6.567714405409693867 ) ) ;
#12369 = VERTEX_POINT ( 'NONE', #762 ) ;
#12370 = DIRECTION ( 'NONE',  ( 1.000000000000000000, 0.000000000000000000, -2.168404344971007882E-16 ) ) ;
#12371 = CARTESIAN_POINT ( 'NONE',  ( 19.99999999999999645, -6.310777386698718239, 1.552768423021305022 ) ) ;
#12372 = STYLED_ITEM ( 'NONE', ( #7041 ), #11261 ) ;
#12373 = AXIS2_PLACEMENT_3D ( 'NONE', #11630, #11509, #5825 ) ;
#12374 = DIRECTION ( 'NONE',  ( -3.437775699846489820E-17, -0.2951046417778627751, -0.9554649393887560960 ) ) ;
#12375 = DIRECTION ( 'NONE',  ( -1.140150527077241873E-30, 0.000000000000000000, 1.000000000000000000 ) ) ;
#12376 = ORIENTED_EDGE ( 'NONE', *, *, #10714, .F. ) ;
#12377 = ORIENTED_EDGE ( 'NONE', *, *, #2569, .T. ) ;
#12378 = LINE ( 'NONE', #11405, #61 ) ;
#12379 = COLOUR_RGB ( '', 0.08235294, 0.09019608, 0.10196078) ;
#12380 = B_SPLINE_CURVE_WITH_KNOTS ( 'NONE', 3,
 ( #10771, #10708, #9671, #2016 ),
 .UNSPECIFIED., .F., .F.,
 ( 4, 4 ),
 ( 0.000000000000000000, 0.002452478801916361563 ),
 .UNSPECIFIED. ) ;
#12381 = CARTESIAN_POINT ( 'NONE',  ( -4.197393957002295117, -8.025123413315649349E-14, -3.503767560748944021 ) ) ;
#12382 = DIRECTION ( 'NONE',  ( -1.000000000000000000, 1.010728034814421376E-30, 1.090846720500930387E-30 ) ) ;
#12383 = ADVANCED_FACE ( 'NONE', ( #4695 ), #8619, .T. ) ;
#12384 = DIRECTION ( 'NONE',  ( -1.140150527077241873E-30, 0.000000000000000000, 1.000000000000000000 ) ) ;
#12385 = VECTOR ( 'NONE', #2749, 1000.000000000000000 ) ;
#12386 = CARTESIAN_POINT ( 'NONE',  ( 9.757359312880696578, 30.00000000000000000, -4.242640687119267007 ) ) ;
#12387 = ORIENTED_EDGE ( 'NONE', *, *, #1075, .F. ) ;
#12388 = CARTESIAN_POINT ( 'NONE',  ( 0.000000000000000000, 5.914787828628547572, 4.446941076999753051 ) ) ;
#12389 = DIRECTION ( 'NONE',  ( 0.000000000000000000, 1.000000000000000000, 0.000000000000000000 ) ) ;
#12390 = AXIS2_PLACEMENT_3D ( 'NONE', #7287, #8308, #5348 ) ;
#12391 = CARTESIAN_POINT ( 'NONE',  ( 19.99999999999999645, -6.459281472512932609, -1.243290685169442966 ) ) ;
#12392 = VECTOR ( 'NONE', #3751, 1000.000000000000000 ) ;
#12393 = ORIENTED_EDGE ( 'NONE', *, *, #2669, .T. ) ;
#12394 = CARTESIAN_POINT ( 'NONE',  ( 0.000000000000000000, 0.000000000000000000, 0.000000000000000000 ) ) ;
#12395 = DIRECTION ( 'NONE',  ( -1.000000000000000000, -1.081682119347366197E-16, 6.938893903907228378E-17 ) ) ;
#12396 = LINE ( 'NONE', #2543, #6941 ) ;
#12397 = CARTESIAN_POINT ( 'NONE',  ( 40.00000000000000711, 16.59466514679920124, -6.965300083364793338 ) ) ;
#12398 = EDGE_CURVE ( 'NONE', #8313, #1734, #5719, .T. ) ;
#12399 = CARTESIAN_POINT ( 'NONE',  ( 14.00000000000000000, 13.00000000000000000, 0.000000000000000000 ) ) ;
#12400 = EDGE_CURVE ( 'NONE', #6000, #6900, #6440, .T. ) ;
#12401 = CARTESIAN_POINT ( 'NONE',  ( -11.83215956619923226, 30.00000000000000000, -4.336808689942017736E-16 ) ) ;
#12402 = VECTOR ( 'NONE', #5670, 1000.000000000000000 ) ;
#12403 = PRESENTATION_STYLE_ASSIGNMENT (( #9469 ) ) ;
#12404 = FACE_OUTER_BOUND ( 'NONE', #9742, .T. ) ;
#12405 = ORIENTED_EDGE ( 'NONE', *, *, #12095, .F. ) ;
#12406 = EDGE_LOOP ( 'NONE', ( #6699, #2288, #7671, #1988 ) ) ;
#12407 = ORIENTED_EDGE ( 'NONE', *, *, #4542, .T. ) ;
#12408 = DIRECTION ( 'NONE',  ( -1.000000000000000000, 1.010728034814421376E-30, 1.090846720500930387E-30 ) ) ;
#12409 = AXIS2_PLACEMENT_3D ( 'NONE', #10667, #4822, #8748 ) ;
#12410 = CARTESIAN_POINT ( 'NONE',  ( 19.99999999999999645, 0.2252065540229667429, 6.573992004634855668 ) ) ;
#12411 = DIRECTION ( 'NONE',  ( 0.000000000000000000, 0.000000000000000000, 1.000000000000000000 ) ) ;
#12412 = CARTESIAN_POINT ( 'NONE',  ( 6.000000000000000000, 49.63999999999998636, -19.00000000000000355 ) ) ;
#12413 = ORIENTED_EDGE ( 'NONE', *, *, #7814, .T. ) ;
#12414 = CYLINDRICAL_SURFACE ( 'NONE', #1336, 6.999999999999999112 ) ;
#12415 = EDGE_CURVE ( 'NONE', #12136, #364, #12378, .T. ) ;
#12416 = CARTESIAN_POINT ( 'NONE',  ( 0.000000000000000000, 0.000000000000000000, 0.000000000000000000 ) ) ;
#12417 = ORIENTED_EDGE ( 'NONE', *, *, #2850, .F. ) ;
#12418 = VECTOR ( 'NONE', #4282, 1000.000000000000000 ) ;
#12419 = ORIENTED_EDGE ( 'NONE', *, *, #10514, .F. ) ;
#12420 = FACE_OUTER_BOUND ( 'NONE', #7070, .T. ) ;
#12421 = VERTEX_POINT ( 'NONE', #7014 ) ;
#12422 = AXIS2_PLACEMENT_3D ( 'NONE', #5707, #7392, #6428 ) ;
#12423 = EDGE_LOOP ( 'NONE', ( #1965, #9163, #2281, #7590 ) ) ;
#12424 =( LENGTH_UNIT ( ) NAMED_UNIT ( * ) SI_UNIT ( .MILLI., .METRE. ) );
#12425 = EDGE_LOOP ( 'NONE', ( #11728, #2627, #892, #5570 ) ) ;
#12426 = LINE ( 'NONE', #7457, #3283 ) ;
#12427 = CARTESIAN_POINT ( 'NONE',  ( 19.99999999999999645, 0.000000000000000000, 0.000000000000000000 ) ) ;
#12428 = EDGE_LOOP ( 'NONE', ( #4097, #1775, #6698, #12387 ) ) ;
#12429 = DIRECTION ( 'NONE',  ( -1.000000000000000000, 1.010728034814421376E-30, 1.090846720500930387E-30 ) ) ;
#12430 = CARTESIAN_POINT ( 'NONE',  ( 11.00000000000001599, 19.99999999999999645, 14.15000000000002878 ) ) ;
#12431 = EDGE_CURVE ( 'NONE', #6622, #6552, #6654, .T. ) ;
#12432 = CARTESIAN_POINT ( 'NONE',  ( 2.000000000000001776, 0.000000000000000000, 0.000000000000000000 ) ) ;
#12433 = ADVANCED_FACE ( 'NONE', ( #7964 ), #7845, .F. ) ;
#12434 = CARTESIAN_POINT ( 'NONE',  ( -11.83215956619923226, -30.00000000000000000, -4.336808689942017736E-16 ) ) ;
#12435 = ORIENTED_EDGE ( 'NONE', *, *, #9778, .T. ) ;
#12436 = AXIS2_PLACEMENT_3D ( 'NONE', #3755, #3102, #3632 ) ;
#12437 = VERTEX_POINT ( 'NONE', #10926 ) ;
#12438 = DIRECTION ( 'NONE',  ( -1.000000000000000000, 1.010728034814421376E-30, 1.090846720500930387E-30 ) ) ;
#12439 = EDGE_CURVE ( 'NONE', #7265, #9407, #1082, .T. ) ;
#12440 = CARTESIAN_POINT ( 'NONE',  ( 0.000000000000000000, 0.000000000000000000, 0.000000000000000000 ) ) ;
#12441 = ORIENTED_EDGE ( 'NONE', *, *, #5960, .T. ) ;
#12442 = CARTESIAN_POINT ( 'NONE',  ( -10.00000000000000178, 0.000000000000000000, 0.000000000000000000 ) ) ;
#12443 = AXIS2_PLACEMENT_3D ( 'NONE', #6664, #12591, #10569 ) ;
#12444 = CARTESIAN_POINT ( 'NONE',  ( 19.99999999999999645, 3.908107171477180675, 5.192658214849959819 ) ) ;
#12445 = LINE ( 'NONE', #12508, #8732 ) ;
#12446 = LINE ( 'NONE', #9578, #10052 ) ;
#12447 = ORIENTED_EDGE ( 'NONE', *, *, #2169, .F. ) ;
#12448 = DIRECTION ( 'NONE',  ( 1.000000000000000000, 0.000000000000000000, 0.000000000000000000 ) ) ;
#12449 = AXIS2_PLACEMENT_3D ( 'NONE', #8183, #10157, #11218 ) ;
#12450 = AXIS2_PLACEMENT_3D ( 'NONE', #6300, #4304, #439 ) ;
#12451 = CARTESIAN_POINT ( 'NONE',  ( 19.99999999999999645, -6.486618105788068966, 0.4009819817179238743 ) ) ;
#12452 =( LENGTH_UNIT ( ) NAMED_UNIT ( * ) SI_UNIT ( .MILLI., .METRE. ) );
#12453 = DIRECTION ( 'NONE',  ( -1.000000000000000000, 1.010728034814421376E-30, 1.090846720500930387E-30 ) ) ;
#12454 = ORIENTED_EDGE ( 'NONE', *, *, #5398, .F. ) ;
#12455 = CYLINDRICAL_SURFACE ( 'NONE', #8702, 10.00000000000000000 ) ;
#12456 = DIRECTION ( 'NONE',  ( -1.000000000000000000, 1.010728034814421376E-30, 1.090846720500930387E-30 ) ) ;
#12458 = DIRECTION ( 'NONE',  ( 0.000000000000000000, -1.000000000000000000, 0.000000000000000000 ) ) ;
#12457 = CIRCLE ( 'NONE', #2161, 4.000000000000000000 ) ;
#12459 = FACE_OUTER_BOUND ( 'NONE', #9869, .T. ) ;
#12460 = AXIS2_PLACEMENT_3D ( 'NONE', #5577, #2625, #7447 ) ;
#12461 = CARTESIAN_POINT ( 'NONE',  ( 40.00000000000000711, 10.25912655421750763, -11.14847175327133577 ) ) ;
#12462 = DIRECTION ( 'NONE',  ( 7.272311470006191196E-31, 0.3513748240813434620, -0.9362348706397368714 ) ) ;
#12463 = CARTESIAN_POINT ( 'NONE',  ( 14.00000000000000000, 30.00000000000000000, 0.000000000000000000 ) ) ;
#12464 = CARTESIAN_POINT ( 'NONE',  ( 0.000000000000000000, 0.000000000000000000, 0.000000000000000000 ) ) ;
#12465 = ORIENTED_EDGE ( 'NONE', *, *, #5652, .T. ) ;
#12466 = CIRCLE ( 'NONE', #8751, 10.00000000000002309 ) ;
#12467 = EDGE_LOOP ( 'NONE', ( #10734, #493 ) ) ;
#12468 = VERTEX_POINT ( 'NONE', #8867 ) ;
#12469 = DIRECTION ( 'NONE',  ( -0.7071067811865355823, 0.000000000000000000, 0.7071067811865595631 ) ) ;
#12470 = PLANE ( 'NONE',  #11037 ) ;
#12471 = CARTESIAN_POINT ( 'NONE',  ( 19.99999999999999645, 2.520781513113643513, 6.075668640744193105 ) ) ;
#12472 = LINE ( 'NONE', #5631, #2610 ) ;
#12473 = ORIENTED_EDGE ( 'NONE', *, *, #1159, .F. ) ;
#12474 = CARTESIAN_POINT ( 'NONE',  ( -15.00000000000000000, 2.632990618166788035E-16, 17.85000000000007958 ) ) ;
#12475 = AXIS2_PLACEMENT_3D ( 'NONE', #12125, #7417, #8250 ) ;
#12476 = PRESENTATION_STYLE_ASSIGNMENT (( #6739 ) ) ;
#12477 = EDGE_LOOP ( 'NONE', ( #5547, #1976, #11048, #6158, #7390, #11459, #10608, #7842, #2158 ) ) ;
#12478 = ORIENTED_EDGE ( 'NONE', *, *, #5431, .F. ) ;
#12479 = DIRECTION ( 'NONE',  ( -1.000000000000000000, 1.010728034814421376E-30, 1.090846720500930387E-30 ) ) ;
#12480 = EDGE_LOOP ( 'NONE', ( #5189, #7058, #2628, #6489 ) ) ;
#12481 = ORIENTED_EDGE ( 'NONE', *, *, #7230, .T. ) ;
#12482 =( NAMED_UNIT ( * ) PLANE_ANGLE_UNIT ( ) SI_UNIT ( $, .RADIAN. ) );
#12483 = EDGE_CURVE ( 'NONE', #825, #276, #6853, .T. ) ;
#12484 = EDGE_CURVE ( 'NONE', #12081, #1191, #4381, .T. ) ;
#12485 = CARTESIAN_POINT ( 'NONE',  ( -1.828356344711643322, -3.563200125723179568, -4.514685608865420807E-16 ) ) ;
#12486 = EDGE_CURVE ( 'NONE', #6460, #8908, #5848, .T. ) ;
#12487 = ORIENTED_EDGE ( 'NONE', *, *, #2093, .F. ) ;
#12488 = CIRCLE ( 'NONE', #4245, 6.499000000000009436 ) ;
#12489 = DIRECTION ( 'NONE',  ( -1.000000000000000000, 1.010728034814421376E-30, 1.090846720500930387E-30 ) ) ;
#12490 = AXIS2_PLACEMENT_3D ( 'NONE', #12410, #7442, #6480 ) ;
#12491 = CARTESIAN_POINT ( 'NONE',  ( 4.200000000000001954, 2.449293598294707893E-16, -2.000000000000018208 ) ) ;
#12492 = ORIENTED_EDGE ( 'NONE', *, *, #12514, .F. ) ;
#12493 = CARTESIAN_POINT ( 'NONE',  ( 0.000000000000000000, -6.453973581750236832, -0.7636923504069602631 ) ) ;
#12494 = CARTESIAN_POINT ( 'NONE',  ( 0.000000000000000000, -3.730839900301502254, -5.321450426182545712 ) ) ;
#12495 = DIRECTION ( 'NONE',  ( -1.000000000000000000, 1.010728034814421376E-30, 1.090846720500930387E-30 ) ) ;
#12496 = AXIS2_PLACEMENT_3D ( 'NONE', #5617, #7804, #9528 ) ;
#12497 = AXIS2_PLACEMENT_3D ( 'NONE', #4399, #8321, #9527 ) ;
#12498 = EDGE_LOOP ( 'NONE', ( #8816, #1328, #668, #12676 ) ) ;
#12499 = ORIENTED_EDGE ( 'NONE', *, *, #2055, .T. ) ;
#12500 = DIRECTION ( 'NONE',  ( 0.000000000000000000, -0.2951046417778627751, -0.9554649393887560960 ) ) ;
#12501 = DIRECTION ( 'NONE',  ( -1.000000000000000000, -1.081682119347362869E-16, 3.143182988685428759E-16 ) ) ;
#12502 = ORIENTED_EDGE ( 'NONE', *, *, #9496, .F. ) ;
#12503 = DIRECTION ( 'NONE',  ( -1.000000000000000000, 1.010728034814421376E-30, 1.090846720500930387E-30 ) ) ;
#12504 = PRODUCT_DEFINITION_FORMATION_WITH_SPECIFIED_SOURCE ( 'ANY', '', #7209, .NOT_KNOWN. ) ;
#12505 = LINE ( 'NONE', #11540, #2448 ) ;
#12506 = VECTOR ( 'NONE', #2174, 1000.000000000000000 ) ;
#12507 = EDGE_CURVE ( 'NONE', #2472, #9566, #7868, .T. ) ;
#12508 = CARTESIAN_POINT ( 'NONE',  ( 20.00000000000000000, 11.34118543499637077, -24.03007857557328464 ) ) ;
#12509 = DIRECTION ( 'NONE',  ( -1.000000000000000000, -1.031065855027150586E-29, 2.218671295934095703E-30 ) ) ;
#12510 = EDGE_LOOP ( 'NONE', ( #12098, #7527 ) ) ;
#12511 = DIRECTION ( 'NONE',  ( -1.000000000000000000, 1.010728034814421376E-30, 1.090846720500930387E-30 ) ) ;
#12512 = VERTEX_POINT ( 'NONE', #7901 ) ;
#12513 = CARTESIAN_POINT ( 'NONE',  ( 19.99999999999999645, -6.459281472512932609, 1.556709314830560853 ) ) ;
#12514 = EDGE_CURVE ( 'NONE', #4835, #8365, #4786, .T. ) ;
#12515 = EDGE_CURVE ( 'NONE', #11656, #4011, #470, .T. ) ;
#12516 = CARTESIAN_POINT ( 'NONE',  ( 20.00000000000000000, 0.000000000000000000, 2.500000000000003553 ) ) ;
#12517 = CARTESIAN_POINT ( 'NONE',  ( -15.00000000000003375, 19.99999999999998579, 14.15000000000002167 ) ) ;
#12518 = LINE ( 'NONE', #779, #10358 ) ;
#12519 = CARTESIAN_POINT ( 'NONE',  ( 1.144235203016661595, 3.958177651039084921, -0.09382832055444986774 ) ) ;
#12520 = DIRECTION ( 'NONE',  ( -1.224646799147352714E-16, -1.177425296209236909E-30, -1.000000000000000000 ) ) ;
#12521 = FACE_OUTER_BOUND ( 'NONE', #11339, .T. ) ;
#12522 = CIRCLE ( 'NONE', #5750, 2.149999999999999023 ) ;
#12523 = CARTESIAN_POINT ( 'NONE',  ( 0.000000000000000000, 4.618802153517012954, -5.000000000000018652 ) ) ;
#12524 = CYLINDRICAL_SURFACE ( 'NONE', #11309, 6.000000000000000000 ) ;
#12525 = UNCERTAINTY_MEASURE_WITH_UNIT (LENGTH_MEASURE( 1.000000000000000082E-05 ), #2366, 'distance_accuracy_value', 'NONE');
#12526 = CARTESIAN_POINT ( 'NONE',  ( 28.99999999999999645, 3.590298071227288829E-15, -1.610000000000000098 ) ) ;
#12527 = VERTEX_POINT ( 'NONE', #11714 ) ;
#12528 = ADVANCED_FACE ( 'NONE', ( #10797 ), #11783, .F. ) ;
#12529 = CIRCLE ( 'NONE', #12118, 2.800000000000003819 ) ;
#12530 = ORIENTED_EDGE ( 'NONE', *, *, #7003, .T. ) ;
#12531 = ORIENTED_EDGE ( 'NONE', *, *, #3163, .F. ) ;
#12532 = ADVANCED_FACE ( 'NONE', ( #176 ), #4889, .T. ) ;
#12533 = CARTESIAN_POINT ( 'NONE',  ( 19.99999999999999645, -5.362766118793823367, -3.671204237728701969 ) ) ;
#12534 = CARTESIAN_POINT ( 'NONE',  ( 0.1999999999999987899, 0.000000000000000000, 0.000000000000000000 ) ) ;
#12535 = DIRECTION ( 'NONE',  ( 0.000000000000000000, 0.000000000000000000, -1.000000000000000000 ) ) ;
#12536 = CARTESIAN_POINT ( 'NONE',  ( 33.61000000000001364, 0.000000000000000000, 2.000000000000000888 ) ) ;
#12537 = ORIENTED_EDGE ( 'NONE', *, *, #10166, .T. ) ;
#12538 = EDGE_CURVE ( 'NONE', #11974, #8622, #6889, .T. ) ;
#12539 = DIRECTION ( 'NONE',  ( -1.000000000000000000, 0.000000000000000000, 0.000000000000000000 ) ) ;
#12540 = FILL_AREA_STYLE_COLOUR ( '', #9040 ) ;
#12541 = ORIENTED_EDGE ( 'NONE', *, *, #2644, .F. ) ;
#12542 = EDGE_LOOP ( 'NONE', ( #11009, #11255 ) ) ;
#12543 = DIRECTION ( 'NONE',  ( -1.000000000000000000, 1.010728034814421376E-30, 1.090846720500930387E-30 ) ) ;
#12544 = ORIENTED_EDGE ( 'NONE', *, *, #4760, .F. ) ;
#12545 = ORIENTED_EDGE ( 'NONE', *, *, #6529, .T. ) ;
#12546 = DIRECTION ( 'NONE',  ( 1.000000000000000000, 0.000000000000000000, 0.000000000000000000 ) ) ;
#12547 = CIRCLE ( 'NONE', #186, 2.800000000000002931 ) ;
#12548 = CARTESIAN_POINT ( 'NONE',  ( 19.99999999999999645, 5.956456411769392112, 2.790827096699012522 ) ) ;
#12549 = AXIS2_PLACEMENT_3D ( 'NONE', #4403, #3454, #11294 ) ;
#12550 = ORIENTED_EDGE ( 'NONE', *, *, #3969, .T. ) ;
#12551 = AXIS2_PLACEMENT_3D ( 'NONE', #12391, #11607, #8505 ) ;
#12552 = EDGE_CURVE ( 'NONE', #9732, #1045, #6227, .T. ) ;
#12553 = CARTESIAN_POINT ( 'NONE',  ( 15.00000000000003375, 12.50000000000000000, 6.000000000000000000 ) ) ;
#12554 = DIRECTION ( 'NONE',  ( 0.000000000000000000, 0.000000000000000000, 1.000000000000000000 ) ) ;
#12555 = ORIENTED_EDGE ( 'NONE', *, *, #658, .T. ) ;
#12556 = DIRECTION ( 'NONE',  ( 3.437775699846481192E-17, 0.2951046417778634967, 0.9554649393887558739 ) ) ;
#12557 = CARTESIAN_POINT ( 'NONE',  ( 19.99999999999997868, 6.557268578288196537, 0.5199208220222073518 ) ) ;
#12558 = EDGE_CURVE ( 'NONE', #11033, #10811, #9699, .T. ) ;
#12559 = CIRCLE ( 'NONE', #10480, 7.400000000000009237 ) ;
#12560 = UNCERTAINTY_MEASURE_WITH_UNIT (LENGTH_MEASURE( 1.000000000000000082E-05 ), #7410, 'distance_accuracy_value', 'NONE');
#12561 = EDGE_CURVE ( 'NONE', #8658, #2488, #8994, .T. ) ;
#12562 = AXIS2_PLACEMENT_3D ( 'NONE', #11223, #10163, #7357 ) ;
#12563 = CONICAL_SURFACE ( 'NONE', #8435, 1.535500000000000087, 1.047197551196590748 ) ;
#12564 = ORIENTED_EDGE ( 'NONE', *, *, #9642, .F. ) ;
#12565 = ORIENTED_EDGE ( 'NONE', *, *, #5335, .F. ) ;
#12566 = CARTESIAN_POINT ( 'NONE',  ( 19.99999999999999645, -6.459281472512945932, 1.243290685169349485 ) ) ;
#12567 = DIRECTION ( 'NONE',  ( 1.000000000000000000, 0.000000000000000000, 0.000000000000000000 ) ) ;
#12568 = ORIENTED_EDGE ( 'NONE', *, *, #10977, .T. ) ;
#12569 = CARTESIAN_POINT ( 'NONE',  ( 0.000000000000000000, -1.773042676681359175, 1.387778780781445676E-14 ) ) ;
#12570 = STYLED_ITEM ( 'NONE', ( #2665 ), #2206 ) ;
#12571 = CIRCLE ( 'NONE', #4748, 2.100000000000000089 ) ;
#12572 = DIRECTION ( 'NONE',  ( 1.140150527077241873E-30, 0.000000000000000000, -1.000000000000000000 ) ) ;
#12573 = CARTESIAN_POINT ( 'NONE',  ( -4.197393957002295117, -0.8151795401431458643, -3.503767560748948906 ) ) ;
#12574 = EDGE_CURVE ( 'NONE', #9626, #229, #4039, .T. ) ;
#12575 = CARTESIAN_POINT ( 'NONE',  ( 8.000000000000000000, 13.00000000000000178, 0.000000000000000000 ) ) ;
#12576 = ORIENTED_EDGE ( 'NONE', *, *, #4151, .T. ) ;
#12578 = CARTESIAN_POINT ( 'NONE',  ( -18.00000000000001421, 29.99999999999999289, 2.000000000000004885 ) ) ;
#12577 = COLOUR_RGB ( '', 0.31764706, 0.68627451, 0.89019608) ;
#12579 = ORIENTED_EDGE ( 'NONE', *, *, #8949, .F. ) ;
#12580 = DIRECTION ( 'NONE',  ( 1.140150527077241873E-30, 0.000000000000000000, -1.000000000000000000 ) ) ;
#12581 = SURFACE_SIDE_STYLE ('',( #6714 ) ) ;
#12582 = EDGE_CURVE ( 'NONE', #8069, #5127, #1489, .T. ) ;
#12583 = DIRECTION ( 'NONE',  ( -1.140150527077241873E-30, 0.000000000000000000, 1.000000000000000000 ) ) ;
#12584 = FACE_OUTER_BOUND ( 'NONE', #7135, .T. ) ;
#12585 = CARTESIAN_POINT ( 'NONE',  ( 8.000000000000000000, -13.00000000000000178, 0.000000000000000000 ) ) ;
#12586 = AXIS2_PLACEMENT_3D ( 'NONE', #6539, #474, #10179 ) ;
#12587 = CARTESIAN_POINT ( 'NONE',  ( 9.999999999999994671, -6.884685972239686258, 2.713134545806031195 ) ) ;
#12588 = DIRECTION ( 'NONE',  ( -1.000000000000000000, -2.206481006425900381E-16, 8.674603474570138454E-17 ) ) ;
#12589 = CARTESIAN_POINT ( 'NONE',  ( 40.00000000000000711, 19.99999999999999645, -12.00000000000000178 ) ) ;
#12590 = EDGE_CURVE ( 'NONE', #2497, #2431, #9693, .T. ) ;
#12591 = DIRECTION ( 'NONE',  ( 1.000000000000000000, 1.081682119347366321E-16, -5.551115123125780237E-17 ) ) ;
#12592 = ADVANCED_FACE ( 'NONE', ( #6354 ), #8092, .T. ) ;
#12593 = DIRECTION ( 'NONE',  ( 0.000000000000000000, 0.000000000000000000, 1.000000000000000000 ) ) ;
#12594 = VECTOR ( 'NONE', #7097, 1000.000000000000000 ) ;
#12595 = LINE ( 'NONE', #4848, #3745 ) ;
#12596 = ORIENTED_EDGE ( 'NONE', *, *, #12123, .F. ) ;
#12597 = VECTOR ( 'NONE', #2536, 1000.000000000000000 ) ;
#12598 = EDGE_CURVE ( 'NONE', #1263, #1849, #8691, .T. ) ;
#12599 = EDGE_LOOP ( 'NONE', ( #6223, #7701, #4823, #4345 ) ) ;
#12600 = VERTEX_POINT ( 'NONE', #4235 ) ;
#12601 = CARTESIAN_POINT ( 'NONE',  ( 40.00000000000000711, 19.99999999999999645, -14.14999999999999503 ) ) ;
#12602 = DIRECTION ( 'NONE',  ( 0.000000000000000000, 0.000000000000000000, 1.000000000000000000 ) ) ;
#12603 = DIRECTION ( 'NONE',  ( -1.000000000000000000, 1.010728034814421376E-30, 1.090846720500930387E-30 ) ) ;
#12604 = LINE ( 'NONE', #6925, #10616 ) ;
#12605 = VERTEX_POINT ( 'NONE', #11259 ) ;
#12606 = FACE_OUTER_BOUND ( 'NONE', #7345, .T. ) ;
#12607 = CIRCLE ( 'NONE', #8275, 6.499000000000006771 ) ;
#12608 = DIRECTION ( 'NONE',  ( 0.000000000000000000, 1.000000000000000000, 0.000000000000000000 ) ) ;
#12609 = ORIENTED_EDGE ( 'NONE', *, *, #2991, .F. ) ;
#12610 = EDGE_LOOP ( 'NONE', ( #10438, #4704, #10136, #8870 ) ) ;
#12611 = PLANE ( 'NONE',  #9 ) ;
#12612 = ORIENTED_EDGE ( 'NONE', *, *, #854, .T. ) ;
#12613 = ORIENTED_EDGE ( 'NONE', *, *, #8383, .F. ) ;
#12614 = VECTOR ( 'NONE', #2653, 1000.000000000000000 ) ;
#12615 = CARTESIAN_POINT ( 'NONE',  ( 40.00000000000000711, 21.12780530657007816, -5.807015647486885257 ) ) ;
#12616 = ORIENTED_EDGE ( 'NONE', *, *, #824, .F. ) ;
#12617 = DIRECTION ( 'NONE',  ( -1.000000000000000000, 0.000000000000000000, 0.000000000000000000 ) ) ;
#12618 = CARTESIAN_POINT ( 'NONE',  ( 14.00000000000000000, -30.00000000000000000, -6.000000000000000000 ) ) ;
#12619 = ORIENTED_EDGE ( 'NONE', *, *, #854, .F. ) ;
#12620 = DIRECTION ( 'NONE',  ( 5.208075316782974243E-17, 0.1525077710325581370, 0.9883022714608525883 ) ) ;
#12621 = CARTESIAN_POINT ( 'NONE',  ( 33.00000000000001421, 81.84122341717352356, -12.68198508464164931 ) ) ;
#12622 = AXIS2_PLACEMENT_3D ( 'NONE', #1572, #9351, #670 ) ;
#12623 = CLOSED_SHELL ( 'NONE', ( #9020, #10086, #3362, #9403, #766, #1296, #9777, #1318, #9173, #4319, #7340, #606, #12284, #10315, #8602, #5809, #3407, #6086, #4740, #7242 ) ) ;
#12624 = EDGE_LOOP ( 'NONE', ( #5913, #12277 ) ) ;
#12625 = ORIENTED_EDGE ( 'NONE', *, *, #12718, .F. ) ;
#12626 = EDGE_LOOP ( 'NONE', ( #6289, #4852, #6254, #2732 ) ) ;
#12627 = CARTESIAN_POINT ( 'NONE',  ( -10.00000000000000178, 0.000000000000000000, 0.000000000000000000 ) ) ;
#12628 = CIRCLE ( 'NONE', #11995, 9.999999999999998224 ) ;
#12629 = CARTESIAN_POINT ( 'NONE',  ( 0.000000000000000000, 0.000000000000000000, 0.000000000000000000 ) ) ;
#12630 = VERTEX_POINT ( 'NONE', #7076 ) ;
#12631 = ADVANCED_FACE ( 'NONE', ( #1396 ), #7465, .F. ) ;
#12632 = CARTESIAN_POINT ( 'NONE',  ( 20.00000000000000000, 21.12780530657007461, -5.807015647486883481 ) ) ;
#12633 = CYLINDRICAL_SURFACE ( 'NONE', #3503, 7.400000000000010125 ) ;
#12634 = CIRCLE ( 'NONE', #488, 10.00000000000000178 ) ;
#12635 = DIRECTION ( 'NONE',  ( -2.465190328815656418E-32, 1.177425296209236734E-30, 1.000000000000000000 ) ) ;
#12636 = ORIENTED_EDGE ( 'NONE', *, *, #6883, .F. ) ;
#12637 = DIRECTION ( 'NONE',  ( 1.000000000000000000, 5.916456789157575403E-31, -1.577021341797098793E-16 ) ) ;
#12638 = ORIENTED_EDGE ( 'NONE', *, *, #2404, .T. ) ;
#12639 = CARTESIAN_POINT ( 'NONE',  ( -4.197393957002295117, -8.025123413315649349E-14, -3.503767560748944021 ) ) ;
#12640 = SHAPE_REPRESENTATION_RELATIONSHIP ( 'NONE' , 'NONE' ,  #1377, #2206 ) ;
#12641 = AXIS2_PLACEMENT_3D ( 'NONE', #10055, #4402, #8326 ) ;
#12642 = DIRECTION ( 'NONE',  ( 0.8191520442889875797, -8.778333957637558005E-33, 0.5735764363510522656 ) ) ;
#12643 = EDGE_CURVE ( 'NONE', #9694, #2472, #495, .T. ) ;
#12644 = AXIS2_PLACEMENT_3D ( 'NONE', #5086, #3236, #7214 ) ;
#12645 = DIRECTION ( 'NONE',  ( 1.154721252774410375E-34, -3.250006781153453386E-32, 1.000000000000000000 ) ) ;
#12646 = CARTESIAN_POINT ( 'NONE',  ( 27.00000000000001421, 81.84122341717352356, -42.68198508464162444 ) ) ;
#12647 = CARTESIAN_POINT ( 'NONE',  ( 19.99999999999997868, -2.720702104306968572, -5.902099716170495114 ) ) ;
#12648 = FACE_OUTER_BOUND ( 'NONE', #748, .T. ) ;
#12649 = LINE ( 'NONE', #6850, #944 ) ;
#12650 = AXIS2_PLACEMENT_3D ( 'NONE', #3758, #11868, #3879 ) ;
#12651 = AXIS2_PLACEMENT_3D ( 'NONE', #49, #12686, #8023 ) ;
#12652 = DIRECTION ( 'NONE',  ( 1.000000000000000000, -1.010728034814421376E-30, -1.090846720500930387E-30 ) ) ;
#12653 = CARTESIAN_POINT ( 'NONE',  ( 19.99999999999997868, 6.359055127044386246, 1.682410996215993881 ) ) ;
#12654 = LINE ( 'NONE', #7686, #5589 ) ;
#12655 = AXIS2_PLACEMENT_3D ( 'NONE', #248, #4182, #3360 ) ;
#12656 = VERTEX_POINT ( 'NONE', #10995 ) ;
#12657 = EDGE_CURVE ( 'NONE', #3780, #10485, #10739, .T. ) ;
#12658 = AXIS2_PLACEMENT_3D ( 'NONE', #5198, #9235, #4165 ) ;
#12659 = ORIENTED_EDGE ( 'NONE', *, *, #6371, .T. ) ;
#12660 = CARTESIAN_POINT ( 'NONE',  ( 3.333333333333355242, -2.694301256218273988, -3.300726591567069601 ) ) ;
#12661 = ADVANCED_FACE ( 'NONE', ( #10202 ), #7271, .T. ) ;
#12662 = CARTESIAN_POINT ( 'NONE',  ( -35.00000000000006395, -30.00000000000000000, 3.000000000000008438 ) ) ;
#12663 = DIRECTION ( 'NONE',  ( 0.000000000000000000, 0.000000000000000000, 1.000000000000000000 ) ) ;
#12664 = DIRECTION ( 'NONE',  ( -1.000000000000000000, 1.010728034814421376E-30, 1.090846720500930387E-30 ) ) ;
#12665 = ORIENTED_EDGE ( 'NONE', *, *, #11215, .F. ) ;
#12666 = EDGE_CURVE ( 'NONE', #9558, #6138, #671, .T. ) ;
#12667 = FACE_OUTER_BOUND ( 'NONE', #9608, .T. ) ;
#12668 = EDGE_CURVE ( 'NONE', #10794, #3780, #2380, .T. ) ;
#12669 = DIRECTION ( 'NONE',  ( 0.000000000000000000, 0.000000000000000000, 1.000000000000000000 ) ) ;
#12670 = ORIENTED_EDGE ( 'NONE', *, *, #916, .T. ) ;
#12671 = AXIS2_PLACEMENT_3D ( 'NONE', #2718, #4078, #3137 ) ;
#12672 = CIRCLE ( 'NONE', #4844, 10.00000000000000178 ) ;
#12673 = VERTEX_POINT ( 'NONE', #11063 ) ;
#12674 = CARTESIAN_POINT ( 'NONE',  ( 0.000000000000000000, 2.180689217871857100, 6.122221454264574092 ) ) ;
#12675 = EDGE_LOOP ( 'NONE', ( #10363, #4900 ) ) ;
#12676 = ORIENTED_EDGE ( 'NONE', *, *, #7433, .T. ) ;
#12677 = DIRECTION ( 'NONE',  ( -1.000000000000000000, 1.010728034814421376E-30, 1.090846720500930387E-30 ) ) ;
#12678 = VERTEX_POINT ( 'NONE', #2313 ) ;
#12679 = EDGE_CURVE ( 'NONE', #1327, #9789, #4590, .T. ) ;
#12680 = CARTESIAN_POINT ( 'NONE',  ( 8.000000000000000000, 30.00000000000000000, -7.347880794884119736E-16 ) ) ;
#12681 = ADVANCED_FACE ( 'NONE', ( #5388 ), #2440, .T. ) ;
#12682 = CARTESIAN_POINT ( 'NONE',  ( 4.000000000000003553, 0.000000000000000000, 0.000000000000000000 ) ) ;
#12683 = ORIENTED_EDGE ( 'NONE', *, *, #758, .T. ) ;
#12684 = AXIS2_PLACEMENT_3D ( 'NONE', #9343, #8451, #4533 ) ;
#12685 = FACE_BOUND ( 'NONE', #2344, .T. ) ;
#12686 = DIRECTION ( 'NONE',  ( -1.000000000000000000, 1.010728034814421376E-30, 1.090846720500930387E-30 ) ) ;
#12687 = VERTEX_POINT ( 'NONE', #12172 ) ;
#12688 = EDGE_LOOP ( 'NONE', ( #243, #8177, #8292, #4388 ) ) ;
#12689 = EDGE_LOOP ( 'NONE', ( #8189, #3367, #162, #6933 ) ) ;
#12690 = VECTOR ( 'NONE', #5575, 1000.000000000000000 ) ;
#12691 = DIRECTION ( 'NONE',  ( -1.000000000000000000, 1.010728034814421376E-30, 1.090846720500930387E-30 ) ) ;
#12692 = VECTOR ( 'NONE', #6430, 1000.000000000000000 ) ;
#12693 = VERTEX_POINT ( 'NONE', #2246 ) ;
#12694 = LINE ( 'NONE', #6954, #11711 ) ;
#12695 = ORIENTED_EDGE ( 'NONE', *, *, #7561, .F. ) ;
#12696 = DIRECTION ( 'NONE',  ( 0.000000000000000000, 0.000000000000000000, 1.000000000000000000 ) ) ;
#12697 = EDGE_CURVE ( 'NONE', #364, #9347, #6102, .T. ) ;
#12698 = EDGE_CURVE ( 'NONE', #6291, #245, #1461, .T. ) ;
#12699 = CARTESIAN_POINT ( 'NONE',  ( -0.1404048886732668089, -4.699864953788076782, -3.686887068327048045 ) ) ;
#12700 = CYLINDRICAL_SURFACE ( 'NONE', #1433, 2.800000000000003819 ) ;
#12701 = ORIENTED_EDGE ( 'NONE', *, *, #3549, .T. ) ;
#12702 = CARTESIAN_POINT ( 'NONE',  ( 9.999999999999994671, -2.171317488608541346, 7.074275960383700657 ) ) ;
#12703 = ORIENTED_EDGE ( 'NONE', *, *, #5856, .T. ) ;
#12704 = CARTESIAN_POINT ( 'NONE',  ( 9.000000000000028422, 30.00000000000000000, 5.000000000000004441 ) ) ;
#12705 = CIRCLE ( 'NONE', #800, 2.000000000000003553 ) ;
#12706 = SURFACE_SIDE_STYLE ('',( #11668 ) ) ;
#12707 = CIRCLE ( 'NONE', #11474, 2.149999999999999023 ) ;
#12708 = LINE ( 'NONE', #4057, #4948 ) ;
#12709 = CARTESIAN_POINT ( 'NONE',  ( 0.000000000000000000, 30.00000000000000000, 0.000000000000000000 ) ) ;
#12710 = DIRECTION ( 'NONE',  ( -1.000000000000000000, 1.010728034814421376E-30, 1.090846720500930387E-30 ) ) ;
#12711 = LINE ( 'NONE', #3877, #5280 ) ;
#12712 = DIRECTION ( 'NONE',  ( 0.000000000000000000, 1.000000000000000000, 0.000000000000000000 ) ) ;
#12713 = CARTESIAN_POINT ( 'NONE',  ( 9.999999999999998224, 0.4528593230175856910, -7.386130139224213131 ) ) ;
#12714 = AXIS2_PLACEMENT_3D ( 'NONE', #2576, #5527, #630 ) ;
#12715 = EDGE_CURVE ( 'NONE', #7976, #9310, #4796, .T. ) ;
#12716 = EDGE_CURVE ( 'NONE', #10532, #11695, #4295, .T. ) ;
#12717 = LINE ( 'NONE', #2937, #3711 ) ;
#12718 = EDGE_CURVE ( 'NONE', #7319, #8682, #3288, .T. ) ;
#12719 = EDGE_CURVE ( 'NONE', #4489, #1584, #4426, .T. ) ;
#12720 = DIRECTION ( 'NONE',  ( -1.000000000000000000, 1.010728034814421376E-30, 1.090846720500930387E-30 ) ) ;
#12721 = VERTEX_POINT ( 'NONE', #2567 ) ;
#12722 = ORIENTED_EDGE ( 'NONE', *, *, #9722, .F. ) ;
#12723 = DIRECTION ( 'NONE',  ( -1.000000000000000000, 1.010728034814421376E-30, 1.090846720500930387E-30 ) ) ;
#12724 = PLANE ( 'NONE',  #2623 ) ;
#12725 = DIRECTION ( 'NONE',  ( 0.000000000000000000, 0.000000000000000000, -1.000000000000000000 ) ) ;
#12726 = DIRECTION ( 'NONE',  ( -1.000000000000000000, 1.010728034814421376E-30, 1.090846720500930387E-30 ) ) ;
#12727 = ORIENTED_EDGE ( 'NONE', *, *, #11706, .T. ) ;
#12728 = LINE ( 'NONE', #6803, #8743 ) ;
#12729 = CARTESIAN_POINT ( 'NONE',  ( 2.000000000000001776, 1.773042676681341856, -3.469446951953614189E-15 ) ) ;
#12730 = CARTESIAN_POINT ( 'NONE',  ( 11.17157287525379772, 30.00000000000000000, -2.828427124746177856 ) ) ;
#12731 = ORIENTED_EDGE ( 'NONE', *, *, #1536, .T. ) ;
#12732 = EDGE_CURVE ( 'NONE', #8146, #2957, #5816, .T. ) ;
#12733 = ORIENTED_EDGE ( 'NONE', *, *, #11820, .F. ) ;
#12734 = DIRECTION ( 'NONE',  ( 0.000000000000000000, 0.000000000000000000, 1.000000000000000000 ) ) ;
#12735 = ORIENTED_EDGE ( 'NONE', *, *, #111, .F. ) ;
#12736 = AXIS2_PLACEMENT_3D ( 'NONE', #4754, #9497, #9559 ) ;
#12737 = VERTEX_POINT ( 'NONE', #11516 ) ;
#12738 = APPLICATION_PROTOCOL_DEFINITION ( 'draft international standard', 'automotive_design', 1998, #6838 ) ;
#12739 = CYLINDRICAL_SURFACE ( 'NONE', #7802, 2.800000000000003819 ) ;
#12740 = EDGE_LOOP ( 'NONE', ( #9567, #3215, #6159, #5137 ) ) ;
#12741 = CARTESIAN_POINT ( 'NONE',  ( -9.000000000000000000, 49.63999999999998636, -19.00000000000000355 ) ) ;
#12742 = EDGE_CURVE ( 'NONE', #7844, #5973, #9105, .T. ) ;
#12743 = CARTESIAN_POINT ( 'NONE',  ( 19.99999999999997868, -0.4733669331951446679, -6.481737787550303942 ) ) ;
#12744 = EDGE_CURVE ( 'NONE', #7136, #8944, #9710, .T. ) ;
#12745 = ORIENTED_EDGE ( 'NONE', *, *, #9372, .T. ) ;
#12746 = AXIS2_PLACEMENT_3D ( 'NONE', #7857, #5920, #9833 ) ;
#12747 = CARTESIAN_POINT ( 'NONE',  ( 0.000000000000000000, 1.528443194675400019, 7.240432404259460775 ) ) ;
#12748 = DIRECTION ( 'NONE',  ( -1.000000000000000000, -1.031065855027150586E-29, 2.218671295934095703E-30 ) ) ;
#12749 = CIRCLE ( 'NONE', #1639, 2.149999999999999023 ) ;
#12750 = NEXT_ASSEMBLY_USAGE_OCCURRENCE ( 'NAUO1', ' ', ' ', #2659, #2904, $ ) ;
#12751 = NEXT_ASSEMBLY_USAGE_OCCURRENCE ( 'NAUO2', ' ', ' ', #2659, #12251, $ ) ;
#12752 = NEXT_ASSEMBLY_USAGE_OCCURRENCE ( 'NAUO3', ' ', ' ', #2659, #6898, $ ) ;
#12753 = NEXT_ASSEMBLY_USAGE_OCCURRENCE ( 'NAUO4', ' ', ' ', #2659, #7290, $ ) ;
#12754 = NEXT_ASSEMBLY_USAGE_OCCURRENCE ( 'NAUO5', ' ', ' ', #2659, #5392, $ ) ;
#12755 = NEXT_ASSEMBLY_USAGE_OCCURRENCE ( 'NAUO6', ' ', ' ', #2659, #5937, $ ) ;
#12756 = NEXT_ASSEMBLY_USAGE_OCCURRENCE ( 'NAUO7', ' ', ' ', #2659, #5164, $ ) ;
#12757 = NEXT_ASSEMBLY_USAGE_OCCURRENCE ( 'NAUO8', ' ', ' ', #2659, #10818, $ ) ;
#12758 = NEXT_ASSEMBLY_USAGE_OCCURRENCE ( 'NAUO9', ' ', ' ', #2659, #2740, $ ) ;
#12759 = NEXT_ASSEMBLY_USAGE_OCCURRENCE ( 'NAUO10', ' ', ' ', #2659, #2740, $ ) ;
#12760 = NEXT_ASSEMBLY_USAGE_OCCURRENCE ( 'NAUO11', ' ', ' ', #2659, #2740, $ ) ;
#12761 = NEXT_ASSEMBLY_USAGE_OCCURRENCE ( 'NAUO12', ' ', ' ', #2659, #9002, $ ) ;
#12762 = NEXT_ASSEMBLY_USAGE_OCCURRENCE ( 'NAUO13', ' ', ' ', #2659, #9002, $ ) ;
#12763 = NEXT_ASSEMBLY_USAGE_OCCURRENCE ( 'NAUO14', ' ', ' ', #2659, #9002, $ ) ;
#12764 = NEXT_ASSEMBLY_USAGE_OCCURRENCE ( 'NAUO15', ' ', ' ', #2659, #4376, $ ) ;
#12765 = NEXT_ASSEMBLY_USAGE_OCCURRENCE ( 'NAUO16', ' ', ' ', #2659, #9002, $ ) ;
ENDSEC;
END-ISO-10303-21;
